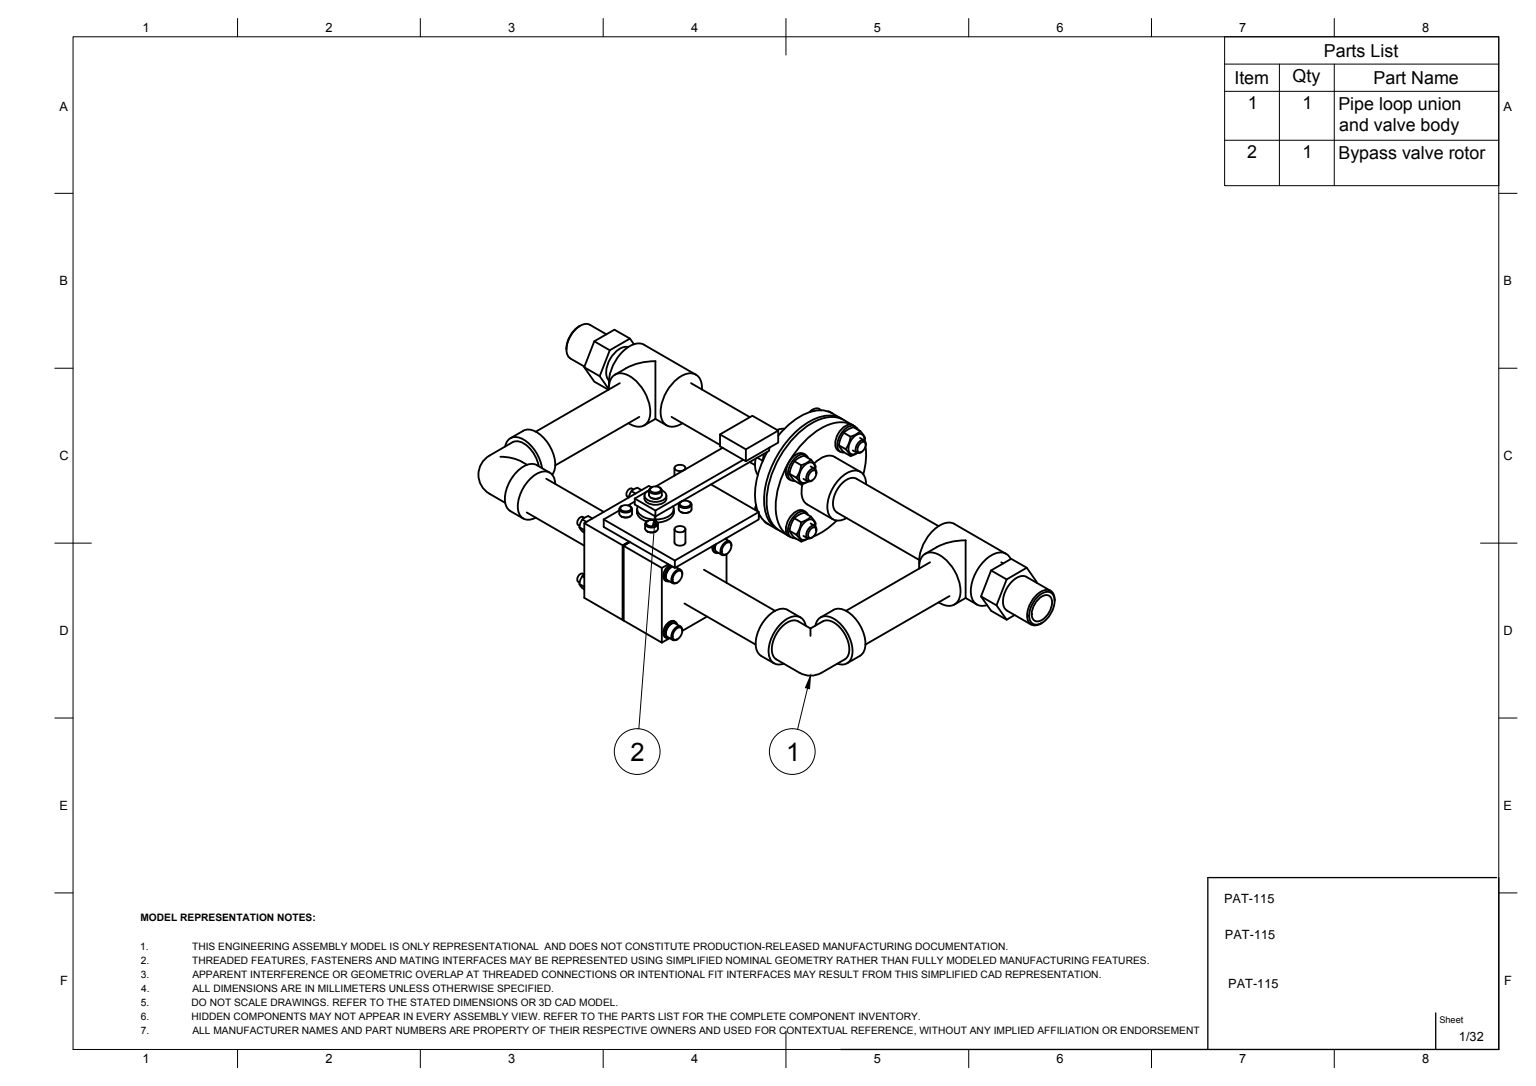
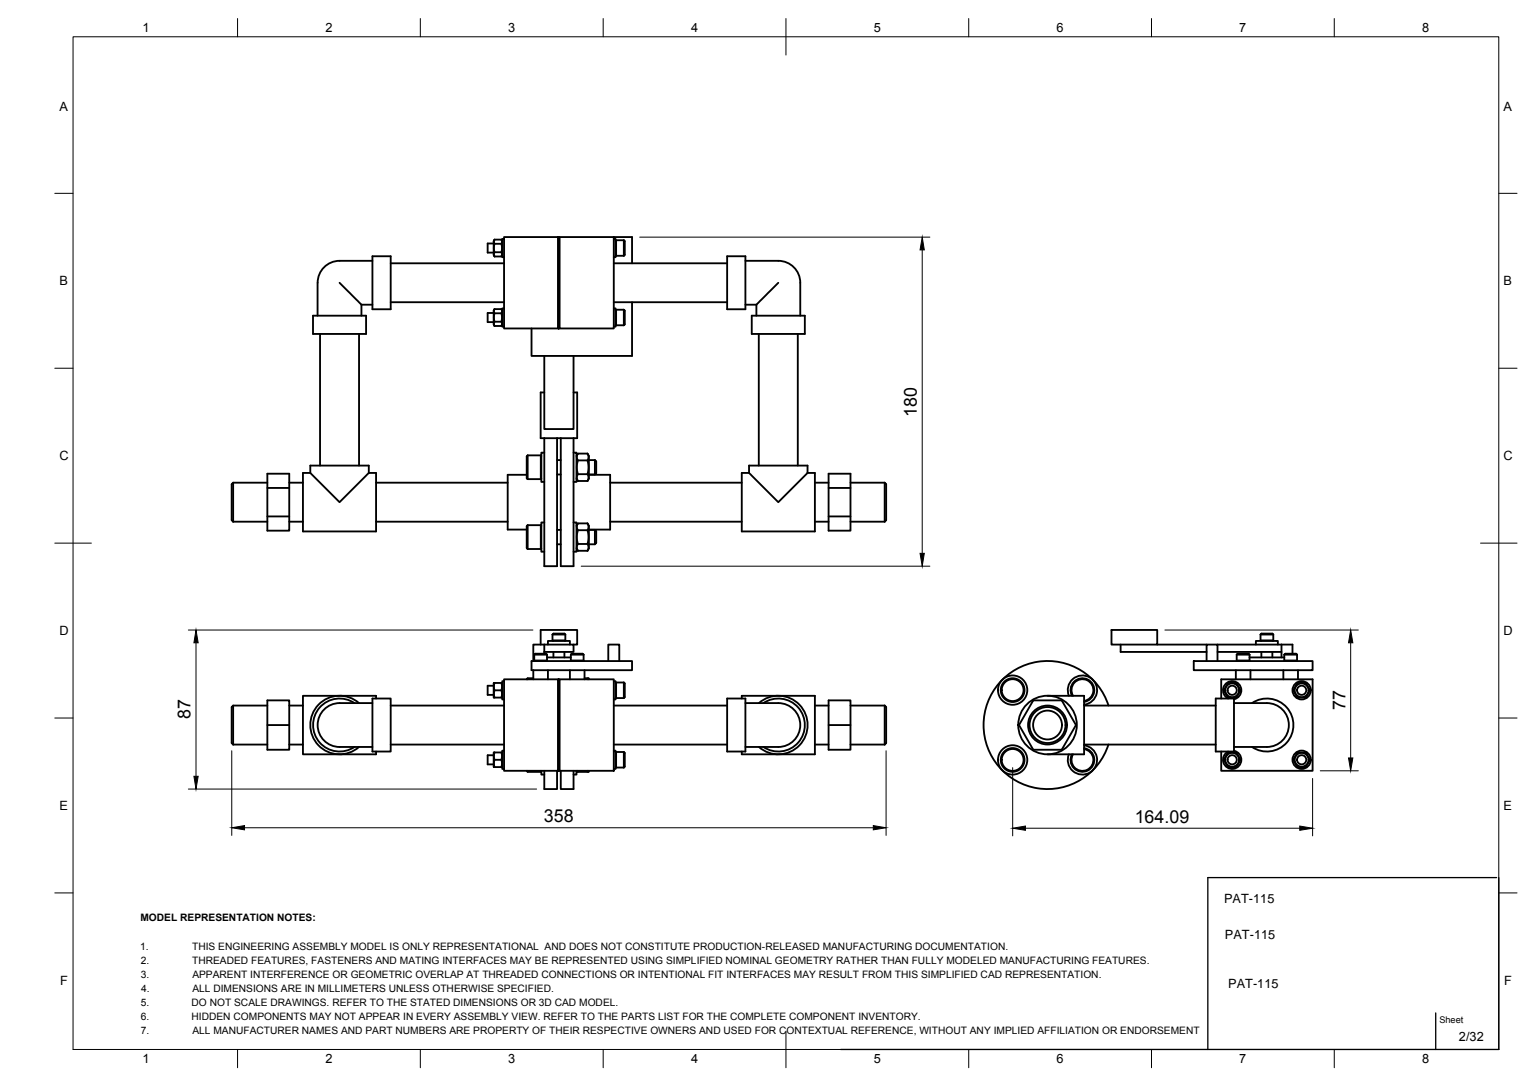
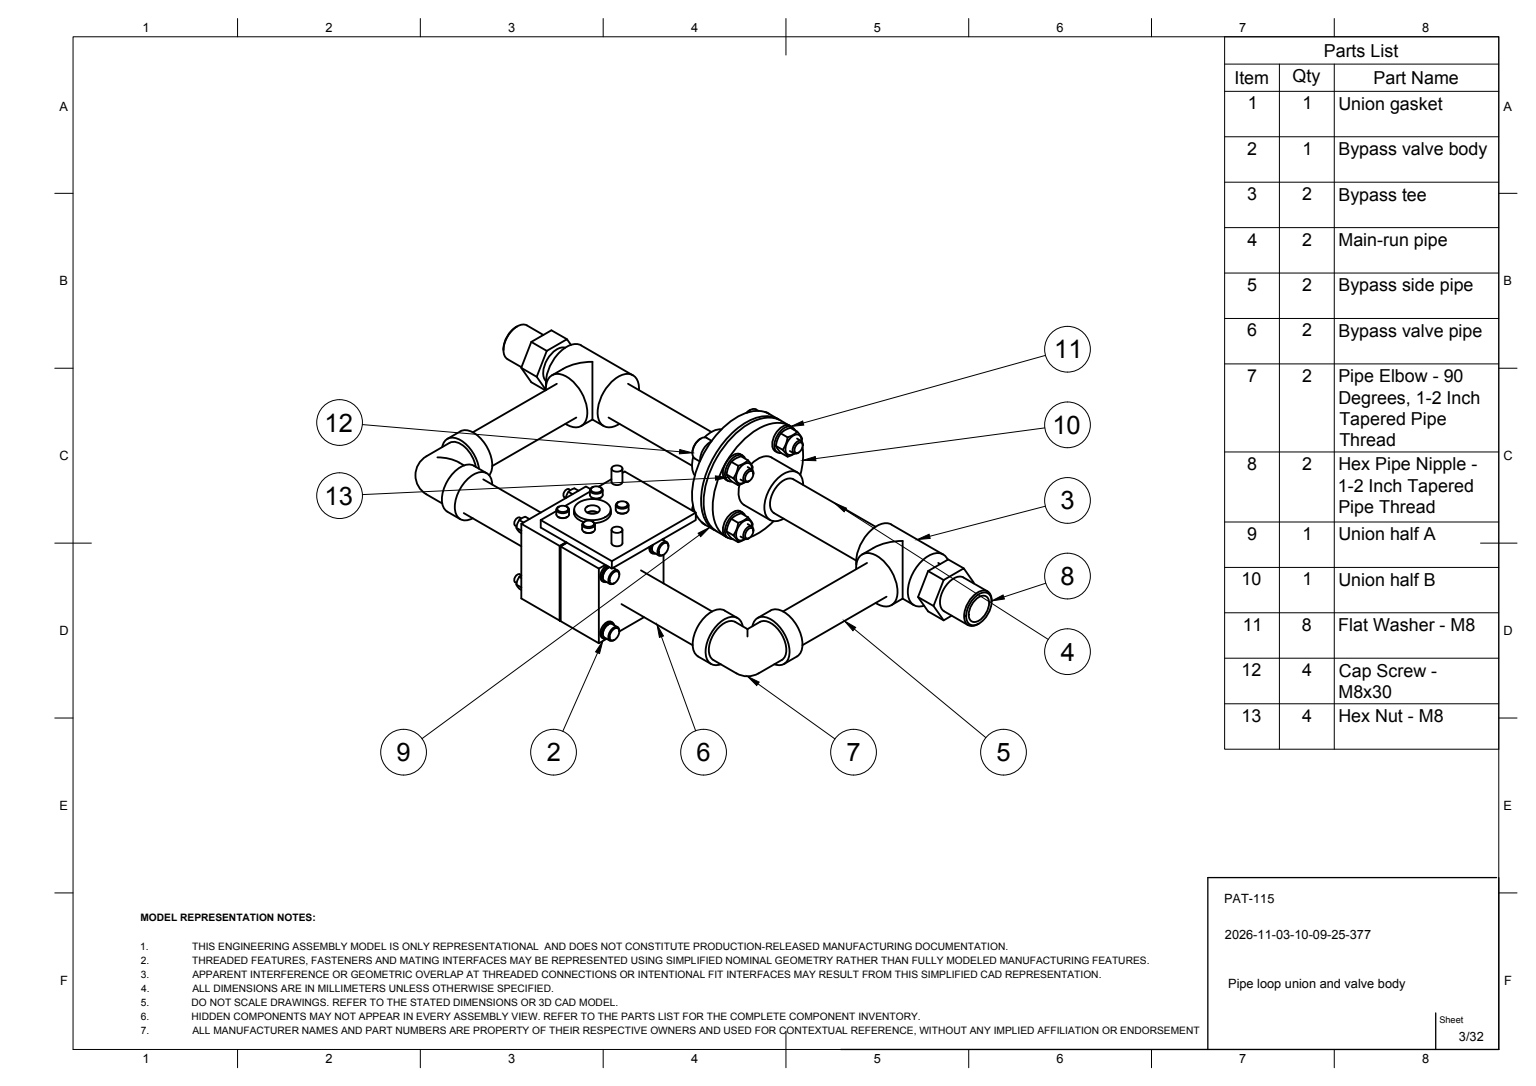
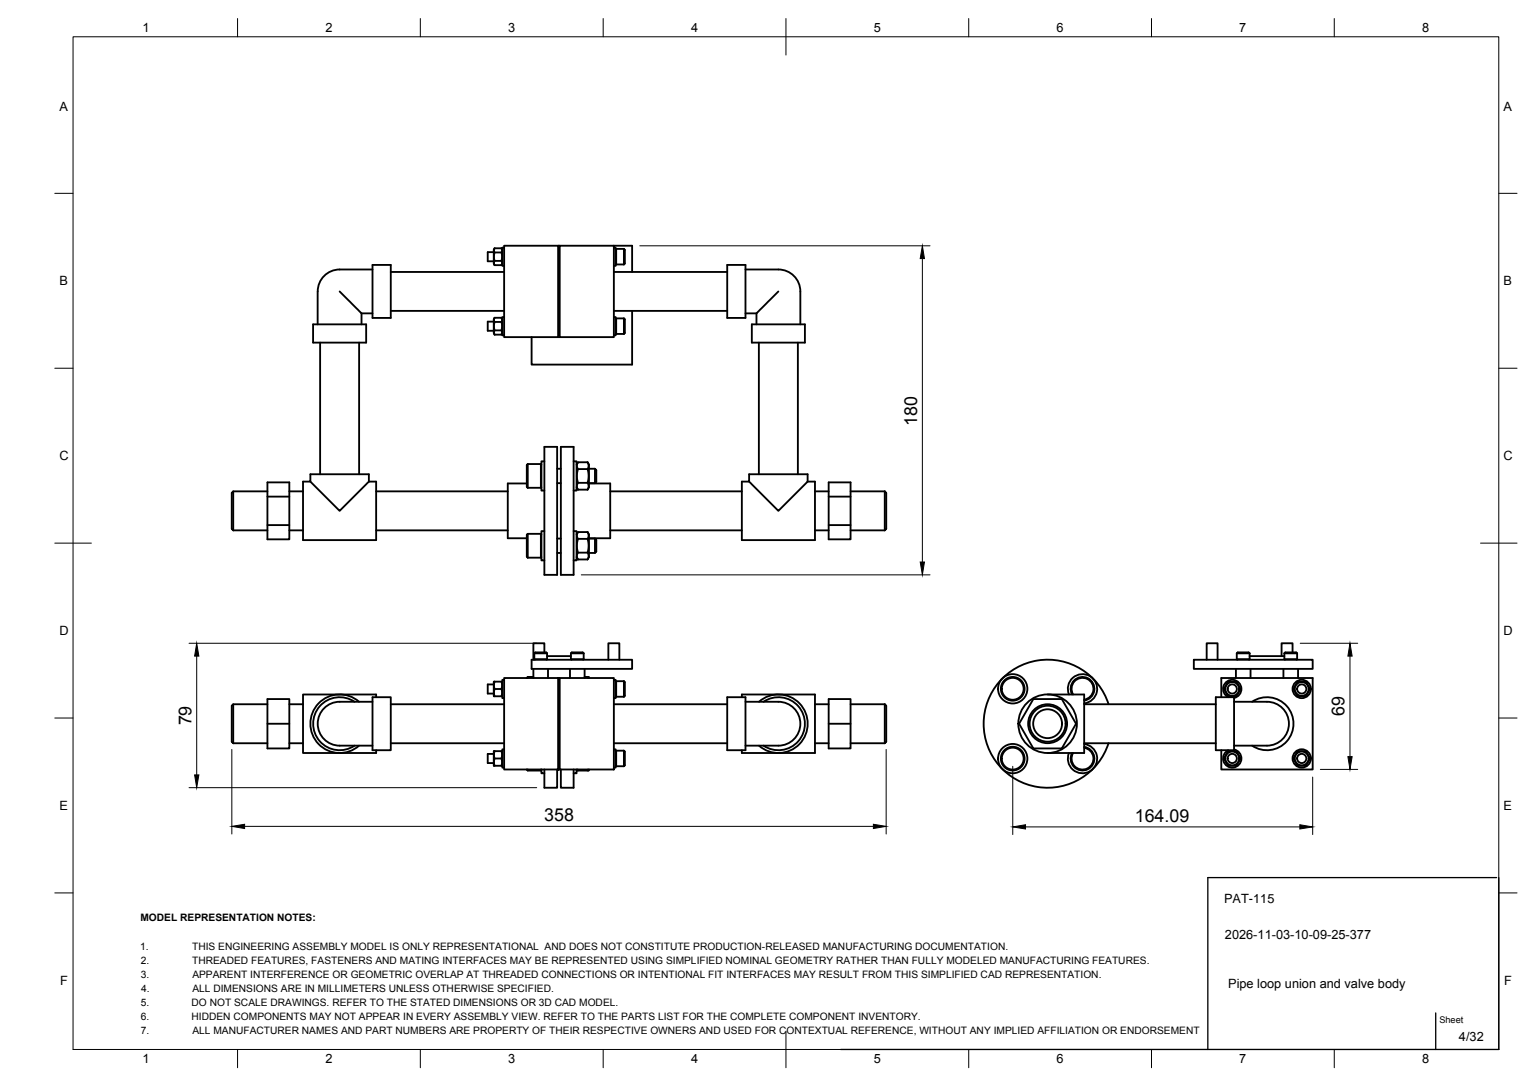
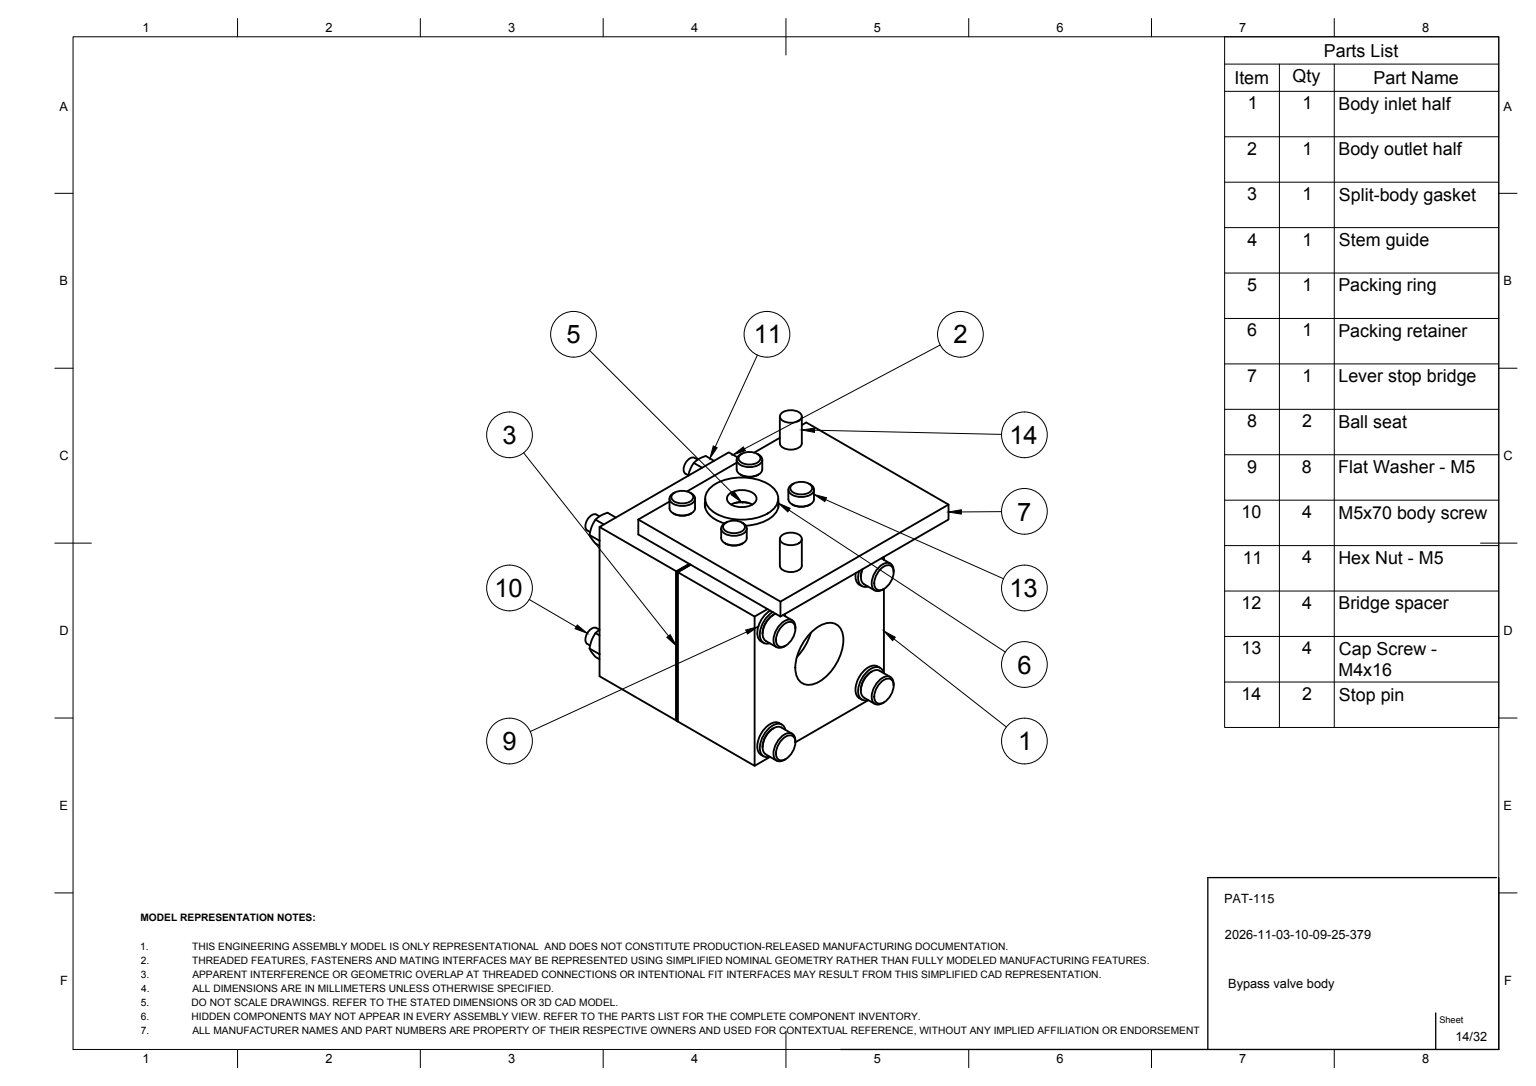
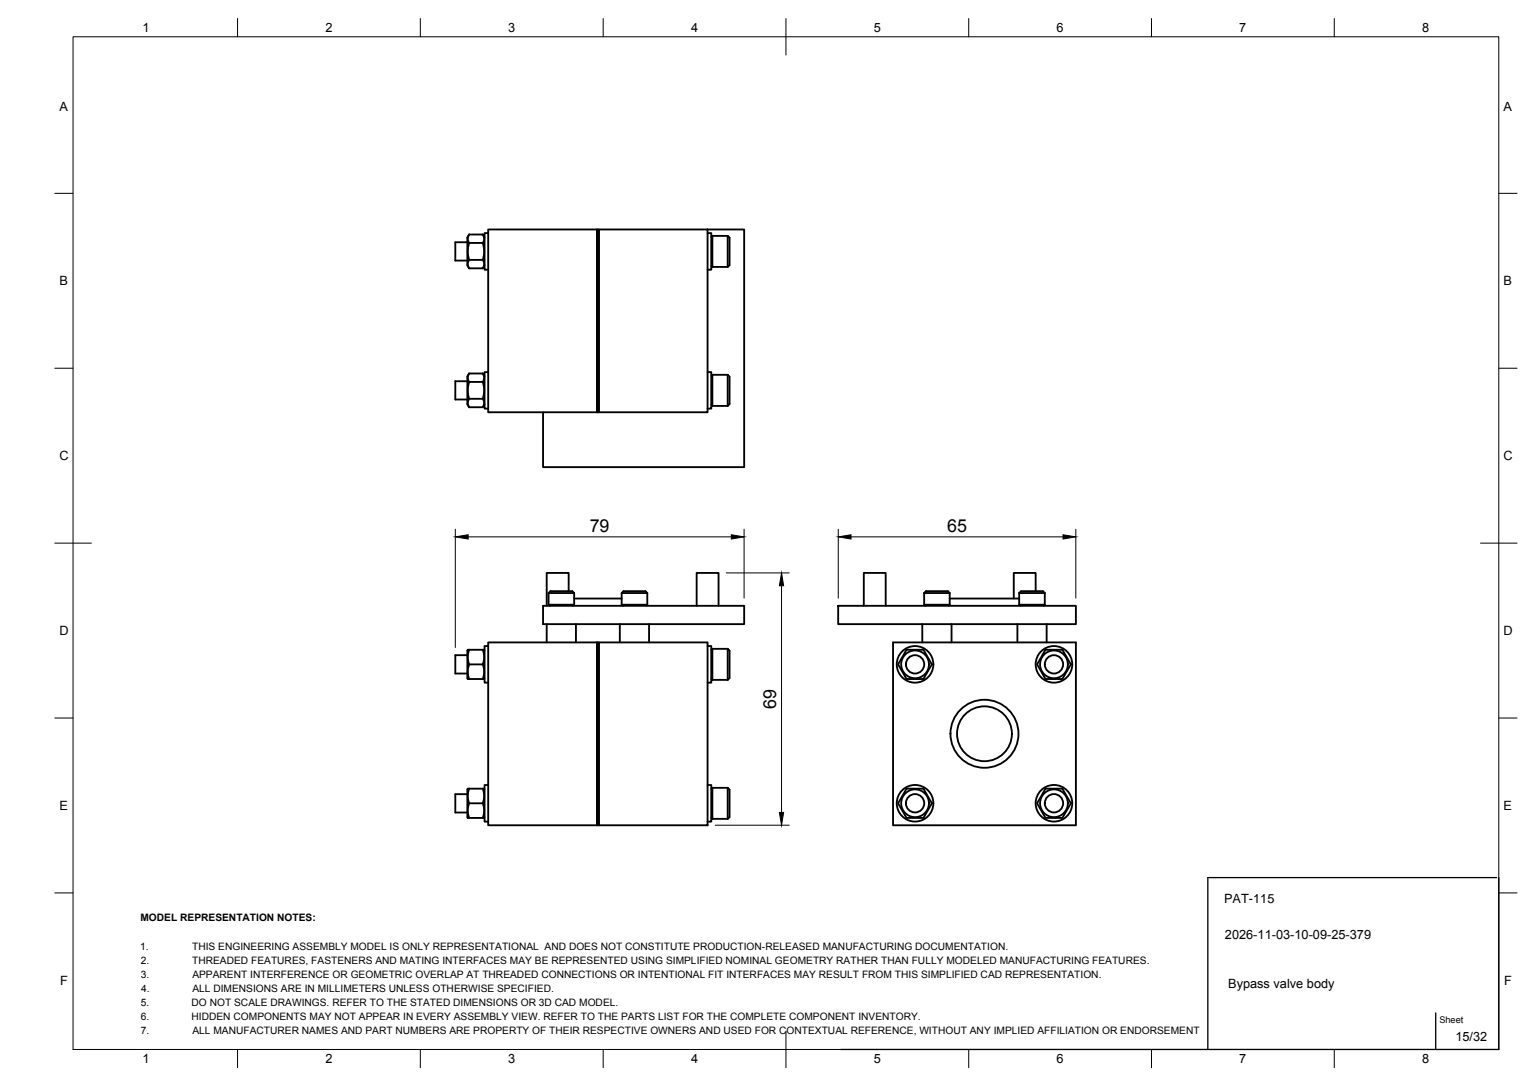
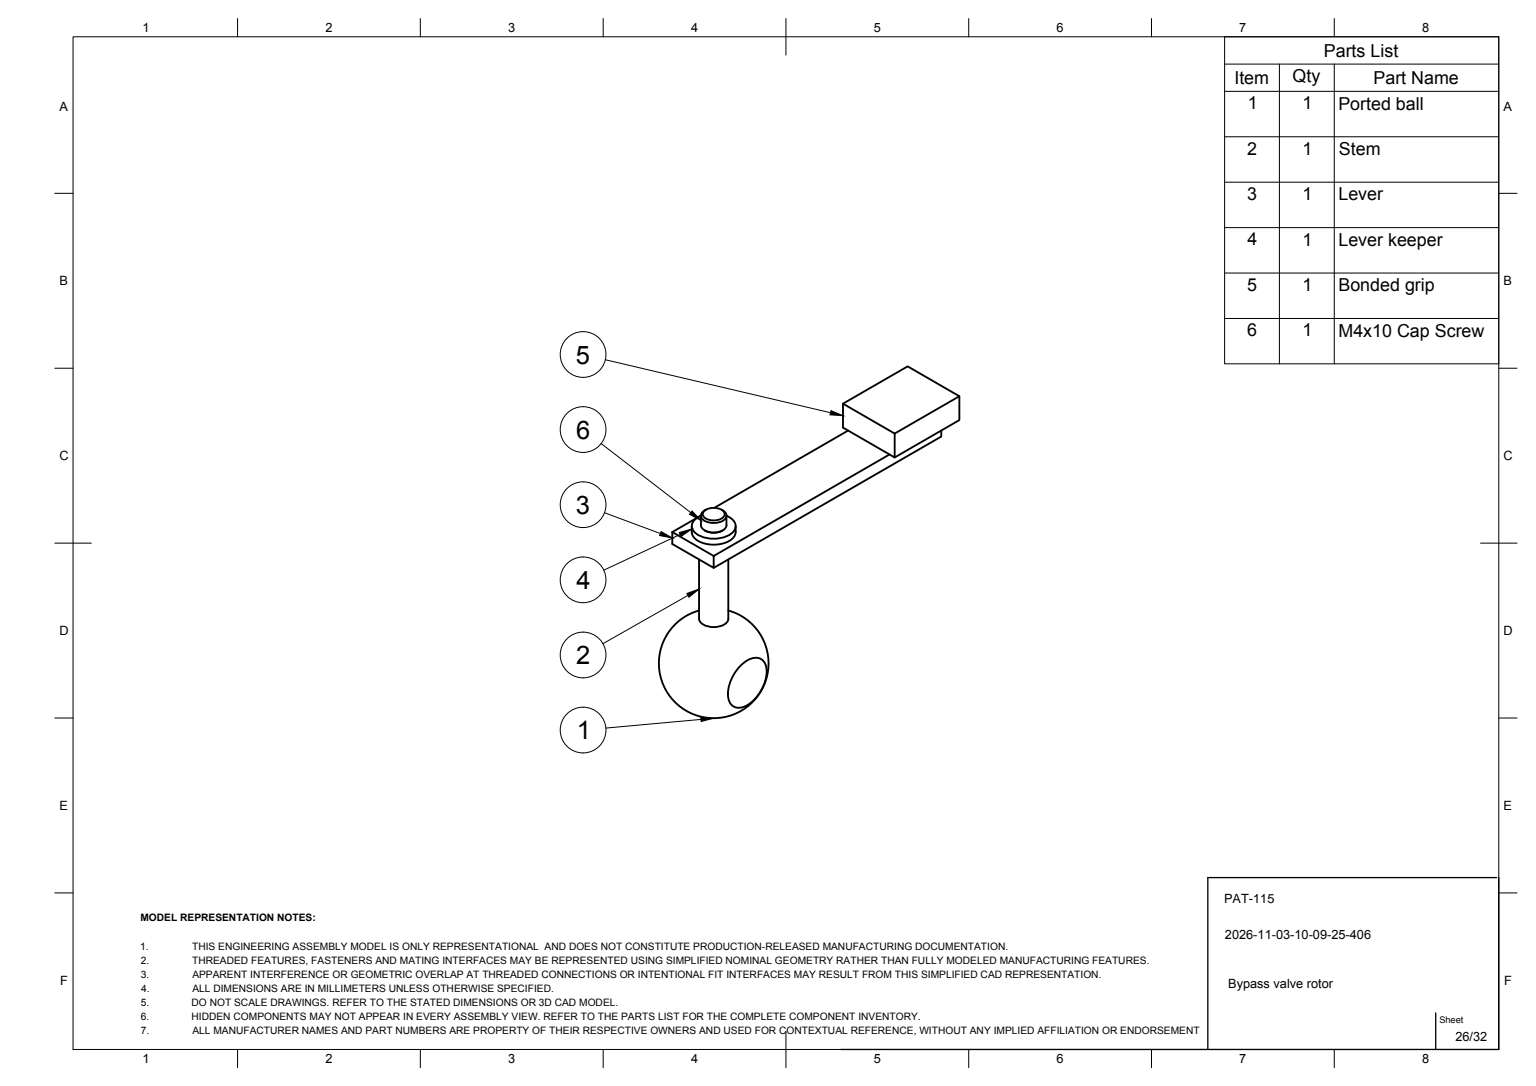
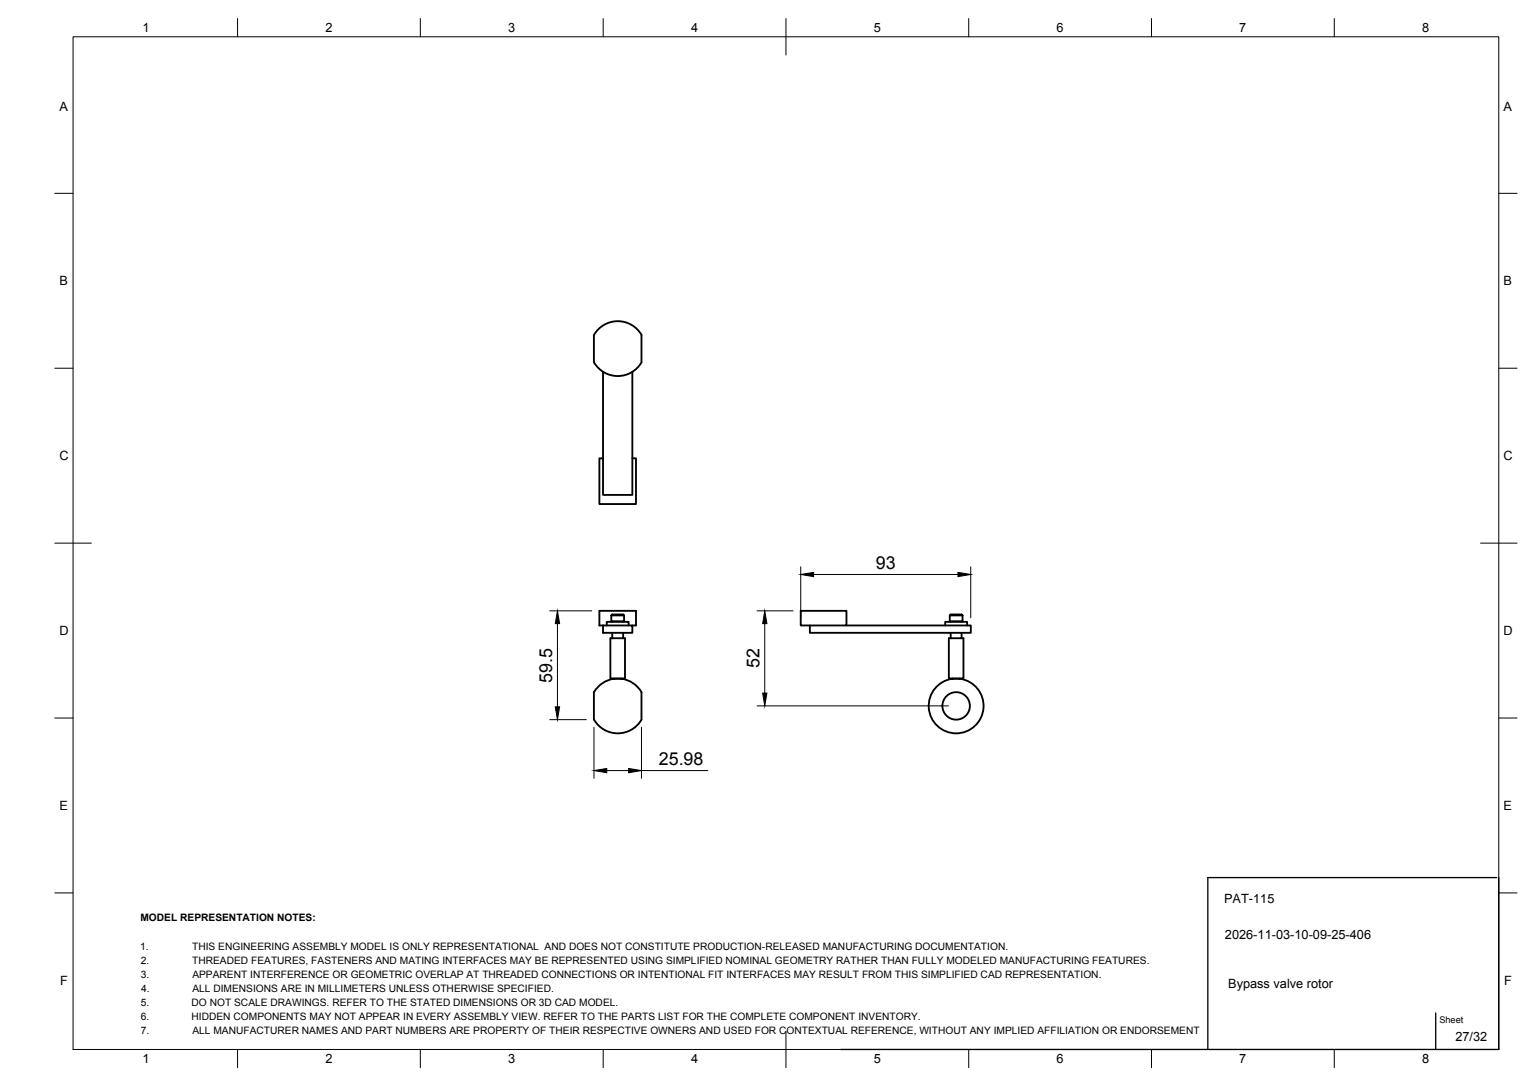
ISO-10303-21;
HEADER;
/* Generated by software containing ST-Developer
 * from STEP Tools, Inc. (www.steptools.com) 
 */

FILE_DESCRIPTION(
/* description */ ('Union bypass pipe loop'),
/* implementation_level */ '2;1');

FILE_NAME(
/* name */ 'PAT-115',
/* time_stamp */ '2026-10-27T21:00:29-07:00',
/* author */ (''),
/* organization */ (''),
/* preprocessor_version */ 'ST-DEVELOPER v20.2',
/* originating_system */ 'Autodesk Translation Framework v15.17.0.0',
/* authorisation */ '');

FILE_SCHEMA (('AUTOMOTIVE_DESIGN { 1 0 10303 214 3 1 1 }'));
ENDSEC;

DATA;
#10=MECHANICAL_DESIGN_GEOMETRIC_PRESENTATION_REPRESENTATION('',(#445,#446,
#447,#448,#449,#450,#451,#452,#453,#454,#455,#456,#457,#458,#459,#460,#461,
#462,#463,#464,#465,#466,#467,#468,#469,#470,#471,#472,#473,#474,#475,#476),
#10095);
#11=ELLIPSE('',#6238,1.31521861300698,0.93);
#12=ELLIPSE('',#6239,1.31521861300698,0.93);
#13=ELLIPSE('',#6241,1.31521861300698,0.93);
#14=ELLIPSE('',#6249,1.11722871427474,0.789999999999999);
#15=ELLIPSE('',#6250,1.11722871427474,0.789999999999999);
#16=ELLIPSE('',#6254,1.11722871427474,0.789999999999999);
#17=ELLIPSE('',#6255,1.11722871427474,0.789999999999999);
#18=ELLIPSE('',#6263,1.11722871427474,0.789999999999999);
#19=ELLIPSE('',#6264,1.11722871427474,0.789999999999999);
#20=ELLIPSE('',#6265,1.11722871427474,0.789999999999999);
#21=ELLIPSE('',#6266,1.11722871427474,0.789999999999999);
#22=ELLIPSE('',#6274,2.26274169979695,1.6);
#23=ELLIPSE('',#6275,2.26274169979695,1.6);
#24=ELLIPSE('',#6277,2.26274169979695,1.6);
#25=ELLIPSE('',#6313,1.11722871427475,0.79);
#26=ELLIPSE('',#6337,1.69705627484771,1.2);
#27=ITEM_DEFINED_TRANSFORMATION($,$,#5908,#6188);
#28=ITEM_DEFINED_TRANSFORMATION($,$,#5951,#6189);
#29=ITEM_DEFINED_TRANSFORMATION($,$,#5994,#6190);
#30=ITEM_DEFINED_TRANSFORMATION($,$,#6021,#6191);
#31=ITEM_DEFINED_TRANSFORMATION($,$,#6034,#6192);
#32=ITEM_DEFINED_TRANSFORMATION($,$,#6038,#6193);
#33=ITEM_DEFINED_TRANSFORMATION($,$,#6051,#6194);
#34=ITEM_DEFINED_TRANSFORMATION($,$,#6081,#6195);
#35=ITEM_DEFINED_TRANSFORMATION($,$,#6081,#6196);
#36=ITEM_DEFINED_TRANSFORMATION($,$,#6120,#6197);
#37=ITEM_DEFINED_TRANSFORMATION($,$,#6092,#6198);
#38=ITEM_DEFINED_TRANSFORMATION($,$,#6120,#6199);
#39=ITEM_DEFINED_TRANSFORMATION($,$,#6131,#6200);
#40=ITEM_DEFINED_TRANSFORMATION($,$,#6120,#6201);
#41=ITEM_DEFINED_TRANSFORMATION($,$,#6092,#6202);
#42=ITEM_DEFINED_TRANSFORMATION($,$,#6120,#6203);
#43=ITEM_DEFINED_TRANSFORMATION($,$,#6131,#6204);
#44=ITEM_DEFINED_TRANSFORMATION($,$,#6120,#6205);
#45=ITEM_DEFINED_TRANSFORMATION($,$,#6092,#6206);
#46=ITEM_DEFINED_TRANSFORMATION($,$,#6120,#6207);
#47=ITEM_DEFINED_TRANSFORMATION($,$,#6131,#6208);
#48=ITEM_DEFINED_TRANSFORMATION($,$,#6120,#6209);
#49=ITEM_DEFINED_TRANSFORMATION($,$,#6092,#6210);
#50=ITEM_DEFINED_TRANSFORMATION($,$,#6120,#6211);
#51=ITEM_DEFINED_TRANSFORMATION($,$,#6131,#6212);
#52=ITEM_DEFINED_TRANSFORMATION($,$,#6147,#6213);
#53=ITEM_DEFINED_TRANSFORMATION($,$,#6156,#6214);
#54=ITEM_DEFINED_TRANSFORMATION($,$,#6147,#6215);
#55=ITEM_DEFINED_TRANSFORMATION($,$,#6156,#6216);
#56=ITEM_DEFINED_TRANSFORMATION($,$,#6147,#6217);
#57=ITEM_DEFINED_TRANSFORMATION($,$,#6156,#6218);
#58=ITEM_DEFINED_TRANSFORMATION($,$,#6147,#6219);
#59=ITEM_DEFINED_TRANSFORMATION($,$,#6156,#6220);
#60=ITEM_DEFINED_TRANSFORMATION($,$,#6182,#6221);
#61=ITEM_DEFINED_TRANSFORMATION($,$,#6182,#6222);
#62=ITEM_DEFINED_TRANSFORMATION($,$,#5907,#6476);
#63=ITEM_DEFINED_TRANSFORMATION($,$,#6223,#6477);
#64=ITEM_DEFINED_TRANSFORMATION($,$,#6232,#6478);
#65=ITEM_DEFINED_TRANSFORMATION($,$,#6284,#6479);
#66=ITEM_DEFINED_TRANSFORMATION($,$,#6293,#6480);
#67=ITEM_DEFINED_TRANSFORMATION($,$,#6302,#6481);
#68=ITEM_DEFINED_TRANSFORMATION($,$,#6232,#6482);
#69=ITEM_DEFINED_TRANSFORMATION($,$,#6284,#6483);
#70=ITEM_DEFINED_TRANSFORMATION($,$,#6293,#6484);
#71=ITEM_DEFINED_TRANSFORMATION($,$,#6302,#6485);
#72=ITEM_DEFINED_TRANSFORMATION($,$,#6311,#6486);
#73=ITEM_DEFINED_TRANSFORMATION($,$,#6311,#6487);
#74=ITEM_DEFINED_TRANSFORMATION($,$,#6351,#6488);
#75=ITEM_DEFINED_TRANSFORMATION($,$,#6351,#6489);
#76=ITEM_DEFINED_TRANSFORMATION($,$,#6375,#6490);
#77=ITEM_DEFINED_TRANSFORMATION($,$,#6400,#6491);
#78=ITEM_DEFINED_TRANSFORMATION($,$,#6451,#6492);
#79=ITEM_DEFINED_TRANSFORMATION($,$,#6425,#6493);
#80=ITEM_DEFINED_TRANSFORMATION($,$,#6451,#6494);
#81=ITEM_DEFINED_TRANSFORMATION($,$,#6460,#6495);
#82=ITEM_DEFINED_TRANSFORMATION($,$,#6451,#6496);
#83=ITEM_DEFINED_TRANSFORMATION($,$,#6425,#6497);
#84=ITEM_DEFINED_TRANSFORMATION($,$,#6451,#6498);
#85=ITEM_DEFINED_TRANSFORMATION($,$,#6460,#6499);
#86=ITEM_DEFINED_TRANSFORMATION($,$,#6451,#6500);
#87=ITEM_DEFINED_TRANSFORMATION($,$,#6425,#6501);
#88=ITEM_DEFINED_TRANSFORMATION($,$,#6451,#6502);
#89=ITEM_DEFINED_TRANSFORMATION($,$,#6460,#6503);
#90=ITEM_DEFINED_TRANSFORMATION($,$,#6451,#6504);
#91=ITEM_DEFINED_TRANSFORMATION($,$,#6425,#6505);
#92=ITEM_DEFINED_TRANSFORMATION($,$,#6451,#6506);
#93=ITEM_DEFINED_TRANSFORMATION($,$,#6460,#6507);
#94=ITEM_DEFINED_TRANSFORMATION($,$,#6509,#6611);
#95=ITEM_DEFINED_TRANSFORMATION($,$,#6525,#6612);
#96=ITEM_DEFINED_TRANSFORMATION($,$,#6560,#6613);
#97=ITEM_DEFINED_TRANSFORMATION($,$,#6571,#6614);
#98=ITEM_DEFINED_TRANSFORMATION($,$,#6580,#6615);
#99=ITEM_DEFINED_TRANSFORMATION($,$,#6587,#6616);
#100=ITEM_DEFINED_TRANSFORMATION($,$,#5906,#6617);
#101=ITEM_DEFINED_TRANSFORMATION($,$,#6508,#6618);
#102=(
REPRESENTATION_RELATIONSHIP($,$,#10250,#10249)
REPRESENTATION_RELATIONSHIP_WITH_TRANSFORMATION(#27)
SHAPE_REPRESENTATION_RELATIONSHIP()
);
#103=(
REPRESENTATION_RELATIONSHIP($,$,#10251,#10249)
REPRESENTATION_RELATIONSHIP_WITH_TRANSFORMATION(#28)
SHAPE_REPRESENTATION_RELATIONSHIP()
);
#104=(
REPRESENTATION_RELATIONSHIP($,$,#10252,#10249)
REPRESENTATION_RELATIONSHIP_WITH_TRANSFORMATION(#29)
SHAPE_REPRESENTATION_RELATIONSHIP()
);
#105=(
REPRESENTATION_RELATIONSHIP($,$,#10253,#10249)
REPRESENTATION_RELATIONSHIP_WITH_TRANSFORMATION(#30)
SHAPE_REPRESENTATION_RELATIONSHIP()
);
#106=(
REPRESENTATION_RELATIONSHIP($,$,#10254,#10249)
REPRESENTATION_RELATIONSHIP_WITH_TRANSFORMATION(#31)
SHAPE_REPRESENTATION_RELATIONSHIP()
);
#107=(
REPRESENTATION_RELATIONSHIP($,$,#10255,#10249)
REPRESENTATION_RELATIONSHIP_WITH_TRANSFORMATION(#32)
SHAPE_REPRESENTATION_RELATIONSHIP()
);
#108=(
REPRESENTATION_RELATIONSHIP($,$,#10256,#10249)
REPRESENTATION_RELATIONSHIP_WITH_TRANSFORMATION(#33)
SHAPE_REPRESENTATION_RELATIONSHIP()
);
#109=(
REPRESENTATION_RELATIONSHIP($,$,#10257,#10249)
REPRESENTATION_RELATIONSHIP_WITH_TRANSFORMATION(#34)
SHAPE_REPRESENTATION_RELATIONSHIP()
);
#110=(
REPRESENTATION_RELATIONSHIP($,$,#10257,#10249)
REPRESENTATION_RELATIONSHIP_WITH_TRANSFORMATION(#35)
SHAPE_REPRESENTATION_RELATIONSHIP()
);
#111=(
REPRESENTATION_RELATIONSHIP($,$,#10259,#10249)
REPRESENTATION_RELATIONSHIP_WITH_TRANSFORMATION(#36)
SHAPE_REPRESENTATION_RELATIONSHIP()
);
#112=(
REPRESENTATION_RELATIONSHIP($,$,#10258,#10249)
REPRESENTATION_RELATIONSHIP_WITH_TRANSFORMATION(#37)
SHAPE_REPRESENTATION_RELATIONSHIP()
);
#113=(
REPRESENTATION_RELATIONSHIP($,$,#10259,#10249)
REPRESENTATION_RELATIONSHIP_WITH_TRANSFORMATION(#38)
SHAPE_REPRESENTATION_RELATIONSHIP()
);
#114=(
REPRESENTATION_RELATIONSHIP($,$,#10260,#10249)
REPRESENTATION_RELATIONSHIP_WITH_TRANSFORMATION(#39)
SHAPE_REPRESENTATION_RELATIONSHIP()
);
#115=(
REPRESENTATION_RELATIONSHIP($,$,#10259,#10249)
REPRESENTATION_RELATIONSHIP_WITH_TRANSFORMATION(#40)
SHAPE_REPRESENTATION_RELATIONSHIP()
);
#116=(
REPRESENTATION_RELATIONSHIP($,$,#10258,#10249)
REPRESENTATION_RELATIONSHIP_WITH_TRANSFORMATION(#41)
SHAPE_REPRESENTATION_RELATIONSHIP()
);
#117=(
REPRESENTATION_RELATIONSHIP($,$,#10259,#10249)
REPRESENTATION_RELATIONSHIP_WITH_TRANSFORMATION(#42)
SHAPE_REPRESENTATION_RELATIONSHIP()
);
#118=(
REPRESENTATION_RELATIONSHIP($,$,#10260,#10249)
REPRESENTATION_RELATIONSHIP_WITH_TRANSFORMATION(#43)
SHAPE_REPRESENTATION_RELATIONSHIP()
);
#119=(
REPRESENTATION_RELATIONSHIP($,$,#10259,#10249)
REPRESENTATION_RELATIONSHIP_WITH_TRANSFORMATION(#44)
SHAPE_REPRESENTATION_RELATIONSHIP()
);
#120=(
REPRESENTATION_RELATIONSHIP($,$,#10258,#10249)
REPRESENTATION_RELATIONSHIP_WITH_TRANSFORMATION(#45)
SHAPE_REPRESENTATION_RELATIONSHIP()
);
#121=(
REPRESENTATION_RELATIONSHIP($,$,#10259,#10249)
REPRESENTATION_RELATIONSHIP_WITH_TRANSFORMATION(#46)
SHAPE_REPRESENTATION_RELATIONSHIP()
);
#122=(
REPRESENTATION_RELATIONSHIP($,$,#10260,#10249)
REPRESENTATION_RELATIONSHIP_WITH_TRANSFORMATION(#47)
SHAPE_REPRESENTATION_RELATIONSHIP()
);
#123=(
REPRESENTATION_RELATIONSHIP($,$,#10259,#10249)
REPRESENTATION_RELATIONSHIP_WITH_TRANSFORMATION(#48)
SHAPE_REPRESENTATION_RELATIONSHIP()
);
#124=(
REPRESENTATION_RELATIONSHIP($,$,#10258,#10249)
REPRESENTATION_RELATIONSHIP_WITH_TRANSFORMATION(#49)
SHAPE_REPRESENTATION_RELATIONSHIP()
);
#125=(
REPRESENTATION_RELATIONSHIP($,$,#10259,#10249)
REPRESENTATION_RELATIONSHIP_WITH_TRANSFORMATION(#50)
SHAPE_REPRESENTATION_RELATIONSHIP()
);
#126=(
REPRESENTATION_RELATIONSHIP($,$,#10260,#10249)
REPRESENTATION_RELATIONSHIP_WITH_TRANSFORMATION(#51)
SHAPE_REPRESENTATION_RELATIONSHIP()
);
#127=(
REPRESENTATION_RELATIONSHIP($,$,#10261,#10249)
REPRESENTATION_RELATIONSHIP_WITH_TRANSFORMATION(#52)
SHAPE_REPRESENTATION_RELATIONSHIP()
);
#128=(
REPRESENTATION_RELATIONSHIP($,$,#10262,#10249)
REPRESENTATION_RELATIONSHIP_WITH_TRANSFORMATION(#53)
SHAPE_REPRESENTATION_RELATIONSHIP()
);
#129=(
REPRESENTATION_RELATIONSHIP($,$,#10261,#10249)
REPRESENTATION_RELATIONSHIP_WITH_TRANSFORMATION(#54)
SHAPE_REPRESENTATION_RELATIONSHIP()
);
#130=(
REPRESENTATION_RELATIONSHIP($,$,#10262,#10249)
REPRESENTATION_RELATIONSHIP_WITH_TRANSFORMATION(#55)
SHAPE_REPRESENTATION_RELATIONSHIP()
);
#131=(
REPRESENTATION_RELATIONSHIP($,$,#10261,#10249)
REPRESENTATION_RELATIONSHIP_WITH_TRANSFORMATION(#56)
SHAPE_REPRESENTATION_RELATIONSHIP()
);
#132=(
REPRESENTATION_RELATIONSHIP($,$,#10262,#10249)
REPRESENTATION_RELATIONSHIP_WITH_TRANSFORMATION(#57)
SHAPE_REPRESENTATION_RELATIONSHIP()
);
#133=(
REPRESENTATION_RELATIONSHIP($,$,#10261,#10249)
REPRESENTATION_RELATIONSHIP_WITH_TRANSFORMATION(#58)
SHAPE_REPRESENTATION_RELATIONSHIP()
);
#134=(
REPRESENTATION_RELATIONSHIP($,$,#10262,#10249)
REPRESENTATION_RELATIONSHIP_WITH_TRANSFORMATION(#59)
SHAPE_REPRESENTATION_RELATIONSHIP()
);
#135=(
REPRESENTATION_RELATIONSHIP($,$,#10263,#10249)
REPRESENTATION_RELATIONSHIP_WITH_TRANSFORMATION(#60)
SHAPE_REPRESENTATION_RELATIONSHIP()
);
#136=(
REPRESENTATION_RELATIONSHIP($,$,#10263,#10249)
REPRESENTATION_RELATIONSHIP_WITH_TRANSFORMATION(#61)
SHAPE_REPRESENTATION_RELATIONSHIP()
);
#137=(
REPRESENTATION_RELATIONSHIP($,$,#10249,#10248)
REPRESENTATION_RELATIONSHIP_WITH_TRANSFORMATION(#62)
SHAPE_REPRESENTATION_RELATIONSHIP()
);
#138=(
REPRESENTATION_RELATIONSHIP($,$,#10264,#10248)
REPRESENTATION_RELATIONSHIP_WITH_TRANSFORMATION(#63)
SHAPE_REPRESENTATION_RELATIONSHIP()
);
#139=(
REPRESENTATION_RELATIONSHIP($,$,#10265,#10248)
REPRESENTATION_RELATIONSHIP_WITH_TRANSFORMATION(#64)
SHAPE_REPRESENTATION_RELATIONSHIP()
);
#140=(
REPRESENTATION_RELATIONSHIP($,$,#10266,#10248)
REPRESENTATION_RELATIONSHIP_WITH_TRANSFORMATION(#65)
SHAPE_REPRESENTATION_RELATIONSHIP()
);
#141=(
REPRESENTATION_RELATIONSHIP($,$,#10267,#10248)
REPRESENTATION_RELATIONSHIP_WITH_TRANSFORMATION(#66)
SHAPE_REPRESENTATION_RELATIONSHIP()
);
#142=(
REPRESENTATION_RELATIONSHIP($,$,#10268,#10248)
REPRESENTATION_RELATIONSHIP_WITH_TRANSFORMATION(#67)
SHAPE_REPRESENTATION_RELATIONSHIP()
);
#143=(
REPRESENTATION_RELATIONSHIP($,$,#10265,#10248)
REPRESENTATION_RELATIONSHIP_WITH_TRANSFORMATION(#68)
SHAPE_REPRESENTATION_RELATIONSHIP()
);
#144=(
REPRESENTATION_RELATIONSHIP($,$,#10266,#10248)
REPRESENTATION_RELATIONSHIP_WITH_TRANSFORMATION(#69)
SHAPE_REPRESENTATION_RELATIONSHIP()
);
#145=(
REPRESENTATION_RELATIONSHIP($,$,#10267,#10248)
REPRESENTATION_RELATIONSHIP_WITH_TRANSFORMATION(#70)
SHAPE_REPRESENTATION_RELATIONSHIP()
);
#146=(
REPRESENTATION_RELATIONSHIP($,$,#10268,#10248)
REPRESENTATION_RELATIONSHIP_WITH_TRANSFORMATION(#71)
SHAPE_REPRESENTATION_RELATIONSHIP()
);
#147=(
REPRESENTATION_RELATIONSHIP($,$,#10269,#10248)
REPRESENTATION_RELATIONSHIP_WITH_TRANSFORMATION(#72)
SHAPE_REPRESENTATION_RELATIONSHIP()
);
#148=(
REPRESENTATION_RELATIONSHIP($,$,#10269,#10248)
REPRESENTATION_RELATIONSHIP_WITH_TRANSFORMATION(#73)
SHAPE_REPRESENTATION_RELATIONSHIP()
);
#149=(
REPRESENTATION_RELATIONSHIP($,$,#10270,#10248)
REPRESENTATION_RELATIONSHIP_WITH_TRANSFORMATION(#74)
SHAPE_REPRESENTATION_RELATIONSHIP()
);
#150=(
REPRESENTATION_RELATIONSHIP($,$,#10270,#10248)
REPRESENTATION_RELATIONSHIP_WITH_TRANSFORMATION(#75)
SHAPE_REPRESENTATION_RELATIONSHIP()
);
#151=(
REPRESENTATION_RELATIONSHIP($,$,#10271,#10248)
REPRESENTATION_RELATIONSHIP_WITH_TRANSFORMATION(#76)
SHAPE_REPRESENTATION_RELATIONSHIP()
);
#152=(
REPRESENTATION_RELATIONSHIP($,$,#10272,#10248)
REPRESENTATION_RELATIONSHIP_WITH_TRANSFORMATION(#77)
SHAPE_REPRESENTATION_RELATIONSHIP()
);
#153=(
REPRESENTATION_RELATIONSHIP($,$,#10274,#10248)
REPRESENTATION_RELATIONSHIP_WITH_TRANSFORMATION(#78)
SHAPE_REPRESENTATION_RELATIONSHIP()
);
#154=(
REPRESENTATION_RELATIONSHIP($,$,#10273,#10248)
REPRESENTATION_RELATIONSHIP_WITH_TRANSFORMATION(#79)
SHAPE_REPRESENTATION_RELATIONSHIP()
);
#155=(
REPRESENTATION_RELATIONSHIP($,$,#10274,#10248)
REPRESENTATION_RELATIONSHIP_WITH_TRANSFORMATION(#80)
SHAPE_REPRESENTATION_RELATIONSHIP()
);
#156=(
REPRESENTATION_RELATIONSHIP($,$,#10275,#10248)
REPRESENTATION_RELATIONSHIP_WITH_TRANSFORMATION(#81)
SHAPE_REPRESENTATION_RELATIONSHIP()
);
#157=(
REPRESENTATION_RELATIONSHIP($,$,#10274,#10248)
REPRESENTATION_RELATIONSHIP_WITH_TRANSFORMATION(#82)
SHAPE_REPRESENTATION_RELATIONSHIP()
);
#158=(
REPRESENTATION_RELATIONSHIP($,$,#10273,#10248)
REPRESENTATION_RELATIONSHIP_WITH_TRANSFORMATION(#83)
SHAPE_REPRESENTATION_RELATIONSHIP()
);
#159=(
REPRESENTATION_RELATIONSHIP($,$,#10274,#10248)
REPRESENTATION_RELATIONSHIP_WITH_TRANSFORMATION(#84)
SHAPE_REPRESENTATION_RELATIONSHIP()
);
#160=(
REPRESENTATION_RELATIONSHIP($,$,#10275,#10248)
REPRESENTATION_RELATIONSHIP_WITH_TRANSFORMATION(#85)
SHAPE_REPRESENTATION_RELATIONSHIP()
);
#161=(
REPRESENTATION_RELATIONSHIP($,$,#10274,#10248)
REPRESENTATION_RELATIONSHIP_WITH_TRANSFORMATION(#86)
SHAPE_REPRESENTATION_RELATIONSHIP()
);
#162=(
REPRESENTATION_RELATIONSHIP($,$,#10273,#10248)
REPRESENTATION_RELATIONSHIP_WITH_TRANSFORMATION(#87)
SHAPE_REPRESENTATION_RELATIONSHIP()
);
#163=(
REPRESENTATION_RELATIONSHIP($,$,#10274,#10248)
REPRESENTATION_RELATIONSHIP_WITH_TRANSFORMATION(#88)
SHAPE_REPRESENTATION_RELATIONSHIP()
);
#164=(
REPRESENTATION_RELATIONSHIP($,$,#10275,#10248)
REPRESENTATION_RELATIONSHIP_WITH_TRANSFORMATION(#89)
SHAPE_REPRESENTATION_RELATIONSHIP()
);
#165=(
REPRESENTATION_RELATIONSHIP($,$,#10274,#10248)
REPRESENTATION_RELATIONSHIP_WITH_TRANSFORMATION(#90)
SHAPE_REPRESENTATION_RELATIONSHIP()
);
#166=(
REPRESENTATION_RELATIONSHIP($,$,#10273,#10248)
REPRESENTATION_RELATIONSHIP_WITH_TRANSFORMATION(#91)
SHAPE_REPRESENTATION_RELATIONSHIP()
);
#167=(
REPRESENTATION_RELATIONSHIP($,$,#10274,#10248)
REPRESENTATION_RELATIONSHIP_WITH_TRANSFORMATION(#92)
SHAPE_REPRESENTATION_RELATIONSHIP()
);
#168=(
REPRESENTATION_RELATIONSHIP($,$,#10275,#10248)
REPRESENTATION_RELATIONSHIP_WITH_TRANSFORMATION(#93)
SHAPE_REPRESENTATION_RELATIONSHIP()
);
#169=(
REPRESENTATION_RELATIONSHIP($,$,#10277,#10276)
REPRESENTATION_RELATIONSHIP_WITH_TRANSFORMATION(#94)
SHAPE_REPRESENTATION_RELATIONSHIP()
);
#170=(
REPRESENTATION_RELATIONSHIP($,$,#10278,#10276)
REPRESENTATION_RELATIONSHIP_WITH_TRANSFORMATION(#95)
SHAPE_REPRESENTATION_RELATIONSHIP()
);
#171=(
REPRESENTATION_RELATIONSHIP($,$,#10279,#10276)
REPRESENTATION_RELATIONSHIP_WITH_TRANSFORMATION(#96)
SHAPE_REPRESENTATION_RELATIONSHIP()
);
#172=(
REPRESENTATION_RELATIONSHIP($,$,#10280,#10276)
REPRESENTATION_RELATIONSHIP_WITH_TRANSFORMATION(#97)
SHAPE_REPRESENTATION_RELATIONSHIP()
);
#173=(
REPRESENTATION_RELATIONSHIP($,$,#10281,#10276)
REPRESENTATION_RELATIONSHIP_WITH_TRANSFORMATION(#98)
SHAPE_REPRESENTATION_RELATIONSHIP()
);
#174=(
REPRESENTATION_RELATIONSHIP($,$,#10282,#10276)
REPRESENTATION_RELATIONSHIP_WITH_TRANSFORMATION(#99)
SHAPE_REPRESENTATION_RELATIONSHIP()
);
#175=(
REPRESENTATION_RELATIONSHIP($,$,#10248,#10247)
REPRESENTATION_RELATIONSHIP_WITH_TRANSFORMATION(#100)
SHAPE_REPRESENTATION_RELATIONSHIP()
);
#176=(
REPRESENTATION_RELATIONSHIP($,$,#10276,#10247)
REPRESENTATION_RELATIONSHIP_WITH_TRANSFORMATION(#101)
SHAPE_REPRESENTATION_RELATIONSHIP()
);
#177=CONTEXT_DEPENDENT_SHAPE_REPRESENTATION(#102,#10153);
#178=CONTEXT_DEPENDENT_SHAPE_REPRESENTATION(#103,#10154);
#179=CONTEXT_DEPENDENT_SHAPE_REPRESENTATION(#104,#10155);
#180=CONTEXT_DEPENDENT_SHAPE_REPRESENTATION(#105,#10156);
#181=CONTEXT_DEPENDENT_SHAPE_REPRESENTATION(#106,#10157);
#182=CONTEXT_DEPENDENT_SHAPE_REPRESENTATION(#107,#10158);
#183=CONTEXT_DEPENDENT_SHAPE_REPRESENTATION(#108,#10159);
#184=CONTEXT_DEPENDENT_SHAPE_REPRESENTATION(#109,#10160);
#185=CONTEXT_DEPENDENT_SHAPE_REPRESENTATION(#110,#10161);
#186=CONTEXT_DEPENDENT_SHAPE_REPRESENTATION(#111,#10162);
#187=CONTEXT_DEPENDENT_SHAPE_REPRESENTATION(#112,#10163);
#188=CONTEXT_DEPENDENT_SHAPE_REPRESENTATION(#113,#10164);
#189=CONTEXT_DEPENDENT_SHAPE_REPRESENTATION(#114,#10165);
#190=CONTEXT_DEPENDENT_SHAPE_REPRESENTATION(#115,#10166);
#191=CONTEXT_DEPENDENT_SHAPE_REPRESENTATION(#116,#10167);
#192=CONTEXT_DEPENDENT_SHAPE_REPRESENTATION(#117,#10168);
#193=CONTEXT_DEPENDENT_SHAPE_REPRESENTATION(#118,#10169);
#194=CONTEXT_DEPENDENT_SHAPE_REPRESENTATION(#119,#10170);
#195=CONTEXT_DEPENDENT_SHAPE_REPRESENTATION(#120,#10171);
#196=CONTEXT_DEPENDENT_SHAPE_REPRESENTATION(#121,#10172);
#197=CONTEXT_DEPENDENT_SHAPE_REPRESENTATION(#122,#10173);
#198=CONTEXT_DEPENDENT_SHAPE_REPRESENTATION(#123,#10174);
#199=CONTEXT_DEPENDENT_SHAPE_REPRESENTATION(#124,#10175);
#200=CONTEXT_DEPENDENT_SHAPE_REPRESENTATION(#125,#10176);
#201=CONTEXT_DEPENDENT_SHAPE_REPRESENTATION(#126,#10177);
#202=CONTEXT_DEPENDENT_SHAPE_REPRESENTATION(#127,#10178);
#203=CONTEXT_DEPENDENT_SHAPE_REPRESENTATION(#128,#10179);
#204=CONTEXT_DEPENDENT_SHAPE_REPRESENTATION(#129,#10180);
#205=CONTEXT_DEPENDENT_SHAPE_REPRESENTATION(#130,#10181);
#206=CONTEXT_DEPENDENT_SHAPE_REPRESENTATION(#131,#10182);
#207=CONTEXT_DEPENDENT_SHAPE_REPRESENTATION(#132,#10183);
#208=CONTEXT_DEPENDENT_SHAPE_REPRESENTATION(#133,#10184);
#209=CONTEXT_DEPENDENT_SHAPE_REPRESENTATION(#134,#10185);
#210=CONTEXT_DEPENDENT_SHAPE_REPRESENTATION(#135,#10186);
#211=CONTEXT_DEPENDENT_SHAPE_REPRESENTATION(#136,#10187);
#212=CONTEXT_DEPENDENT_SHAPE_REPRESENTATION(#137,#10200);
#213=CONTEXT_DEPENDENT_SHAPE_REPRESENTATION(#138,#10201);
#214=CONTEXT_DEPENDENT_SHAPE_REPRESENTATION(#139,#10202);
#215=CONTEXT_DEPENDENT_SHAPE_REPRESENTATION(#140,#10203);
#216=CONTEXT_DEPENDENT_SHAPE_REPRESENTATION(#141,#10204);
#217=CONTEXT_DEPENDENT_SHAPE_REPRESENTATION(#142,#10205);
#218=CONTEXT_DEPENDENT_SHAPE_REPRESENTATION(#143,#10206);
#219=CONTEXT_DEPENDENT_SHAPE_REPRESENTATION(#144,#10207);
#220=CONTEXT_DEPENDENT_SHAPE_REPRESENTATION(#145,#10208);
#221=CONTEXT_DEPENDENT_SHAPE_REPRESENTATION(#146,#10209);
#222=CONTEXT_DEPENDENT_SHAPE_REPRESENTATION(#147,#10210);
#223=CONTEXT_DEPENDENT_SHAPE_REPRESENTATION(#148,#10211);
#224=CONTEXT_DEPENDENT_SHAPE_REPRESENTATION(#149,#10212);
#225=CONTEXT_DEPENDENT_SHAPE_REPRESENTATION(#150,#10213);
#226=CONTEXT_DEPENDENT_SHAPE_REPRESENTATION(#151,#10214);
#227=CONTEXT_DEPENDENT_SHAPE_REPRESENTATION(#152,#10215);
#228=CONTEXT_DEPENDENT_SHAPE_REPRESENTATION(#153,#10216);
#229=CONTEXT_DEPENDENT_SHAPE_REPRESENTATION(#154,#10217);
#230=CONTEXT_DEPENDENT_SHAPE_REPRESENTATION(#155,#10218);
#231=CONTEXT_DEPENDENT_SHAPE_REPRESENTATION(#156,#10219);
#232=CONTEXT_DEPENDENT_SHAPE_REPRESENTATION(#157,#10220);
#233=CONTEXT_DEPENDENT_SHAPE_REPRESENTATION(#158,#10221);
#234=CONTEXT_DEPENDENT_SHAPE_REPRESENTATION(#159,#10222);
#235=CONTEXT_DEPENDENT_SHAPE_REPRESENTATION(#160,#10223);
#236=CONTEXT_DEPENDENT_SHAPE_REPRESENTATION(#161,#10224);
#237=CONTEXT_DEPENDENT_SHAPE_REPRESENTATION(#162,#10225);
#238=CONTEXT_DEPENDENT_SHAPE_REPRESENTATION(#163,#10226);
#239=CONTEXT_DEPENDENT_SHAPE_REPRESENTATION(#164,#10227);
#240=CONTEXT_DEPENDENT_SHAPE_REPRESENTATION(#165,#10228);
#241=CONTEXT_DEPENDENT_SHAPE_REPRESENTATION(#166,#10229);
#242=CONTEXT_DEPENDENT_SHAPE_REPRESENTATION(#167,#10230);
#243=CONTEXT_DEPENDENT_SHAPE_REPRESENTATION(#168,#10231);
#244=CONTEXT_DEPENDENT_SHAPE_REPRESENTATION(#169,#10239);
#245=CONTEXT_DEPENDENT_SHAPE_REPRESENTATION(#170,#10240);
#246=CONTEXT_DEPENDENT_SHAPE_REPRESENTATION(#171,#10241);
#247=CONTEXT_DEPENDENT_SHAPE_REPRESENTATION(#172,#10242);
#248=CONTEXT_DEPENDENT_SHAPE_REPRESENTATION(#173,#10243);
#249=CONTEXT_DEPENDENT_SHAPE_REPRESENTATION(#174,#10244);
#250=CONTEXT_DEPENDENT_SHAPE_REPRESENTATION(#175,#10245);
#251=CONTEXT_DEPENDENT_SHAPE_REPRESENTATION(#176,#10246);
#252=NEXT_ASSEMBLY_USAGE_OCCURRENCE('Body inlet half:2',
'Body inlet half:2','Body inlet half:2',#10286,#10287,
'Body inlet half:2');
#253=NEXT_ASSEMBLY_USAGE_OCCURRENCE('Body outlet half:2',
'Body outlet half:2','Body outlet half:2',#10286,#10288,
'Body outlet half:2');
#254=NEXT_ASSEMBLY_USAGE_OCCURRENCE('Split-body gasket:2',
'Split-body gasket:2','Split-body gasket:2',#10286,#10289,
'Split-body gasket:2');
#255=NEXT_ASSEMBLY_USAGE_OCCURRENCE('Stem guide:2','Stem guide:2',
'Stem guide:2',#10286,#10290,'Stem guide:2');
#256=NEXT_ASSEMBLY_USAGE_OCCURRENCE('Packing ring:2','Packing ring:2',
'Packing ring:2',#10286,#10291,'Packing ring:2');
#257=NEXT_ASSEMBLY_USAGE_OCCURRENCE('Packing retainer:2',
'Packing retainer:2','Packing retainer:2',#10286,#10292,
'Packing retainer:2');
#258=NEXT_ASSEMBLY_USAGE_OCCURRENCE('Lever stop bridge:2',
'Lever stop bridge:2','Lever stop bridge:2',#10286,#10293,
'Lever stop bridge:2');
#259=NEXT_ASSEMBLY_USAGE_OCCURRENCE('Ball seat:2','Ball seat:2',
'Ball seat:2',#10286,#10294,'Ball seat:2');
#260=NEXT_ASSEMBLY_USAGE_OCCURRENCE('Ball seat:3','Ball seat:3',
'Ball seat:3',#10286,#10294,'Ball seat:3');
#261=NEXT_ASSEMBLY_USAGE_OCCURRENCE('Flat Washer - M5:2',
'Flat Washer - M5:2','Flat Washer - M5:2',#10286,#10296,
'Flat Washer - M5:2');
#262=NEXT_ASSEMBLY_USAGE_OCCURRENCE('M5x70 body screw:2',
'M5x70 body screw:2','M5x70 body screw:2',#10286,#10295,
'M5x70 body screw:2');
#263=NEXT_ASSEMBLY_USAGE_OCCURRENCE('Flat Washer - M5:3',
'Flat Washer - M5:3','Flat Washer - M5:3',#10286,#10296,
'Flat Washer - M5:3');
#264=NEXT_ASSEMBLY_USAGE_OCCURRENCE('Hex Nut - M5:2','Hex Nut - M5:2',
'Hex Nut - M5:2',#10286,#10297,'Hex Nut - M5:2');
#265=NEXT_ASSEMBLY_USAGE_OCCURRENCE('Flat Washer - M5:4',
'Flat Washer - M5:4','Flat Washer - M5:4',#10286,#10296,
'Flat Washer - M5:4');
#266=NEXT_ASSEMBLY_USAGE_OCCURRENCE('M5x70 body screw:3',
'M5x70 body screw:3','M5x70 body screw:3',#10286,#10295,
'M5x70 body screw:3');
#267=NEXT_ASSEMBLY_USAGE_OCCURRENCE('Flat Washer - M5:5',
'Flat Washer - M5:5','Flat Washer - M5:5',#10286,#10296,
'Flat Washer - M5:5');
#268=NEXT_ASSEMBLY_USAGE_OCCURRENCE('Hex Nut - M5:3','Hex Nut - M5:3',
'Hex Nut - M5:3',#10286,#10297,'Hex Nut - M5:3');
#269=NEXT_ASSEMBLY_USAGE_OCCURRENCE('Flat Washer - M5:6',
'Flat Washer - M5:6','Flat Washer - M5:6',#10286,#10296,
'Flat Washer - M5:6');
#270=NEXT_ASSEMBLY_USAGE_OCCURRENCE('M5x70 body screw:4',
'M5x70 body screw:4','M5x70 body screw:4',#10286,#10295,
'M5x70 body screw:4');
#271=NEXT_ASSEMBLY_USAGE_OCCURRENCE('Flat Washer - M5:7',
'Flat Washer - M5:7','Flat Washer - M5:7',#10286,#10296,
'Flat Washer - M5:7');
#272=NEXT_ASSEMBLY_USAGE_OCCURRENCE('Hex Nut - M5:4','Hex Nut - M5:4',
'Hex Nut - M5:4',#10286,#10297,'Hex Nut - M5:4');
#273=NEXT_ASSEMBLY_USAGE_OCCURRENCE('Flat Washer - M5:8',
'Flat Washer - M5:8','Flat Washer - M5:8',#10286,#10296,
'Flat Washer - M5:8');
#274=NEXT_ASSEMBLY_USAGE_OCCURRENCE('M5x70 body screw:5',
'M5x70 body screw:5','M5x70 body screw:5',#10286,#10295,
'M5x70 body screw:5');
#275=NEXT_ASSEMBLY_USAGE_OCCURRENCE('Flat Washer - M5:9',
'Flat Washer - M5:9','Flat Washer - M5:9',#10286,#10296,
'Flat Washer - M5:9');
#276=NEXT_ASSEMBLY_USAGE_OCCURRENCE('Hex Nut - M5:5','Hex Nut - M5:5',
'Hex Nut - M5:5',#10286,#10297,'Hex Nut - M5:5');
#277=NEXT_ASSEMBLY_USAGE_OCCURRENCE('Bridge spacer:2','Bridge spacer:2',
'Bridge spacer:2',#10286,#10298,'Bridge spacer:2');
#278=NEXT_ASSEMBLY_USAGE_OCCURRENCE('Cap Screw - M4x16:2',
'Cap Screw - M4x16:2','Cap Screw - M4x16:2',#10286,#10299,
'Cap Screw - M4x16:2');
#279=NEXT_ASSEMBLY_USAGE_OCCURRENCE('Bridge spacer:3','Bridge spacer:3',
'Bridge spacer:3',#10286,#10298,'Bridge spacer:3');
#280=NEXT_ASSEMBLY_USAGE_OCCURRENCE('Cap Screw - M4x16:3',
'Cap Screw - M4x16:3','Cap Screw - M4x16:3',#10286,#10299,
'Cap Screw - M4x16:3');
#281=NEXT_ASSEMBLY_USAGE_OCCURRENCE('Bridge spacer:4','Bridge spacer:4',
'Bridge spacer:4',#10286,#10298,'Bridge spacer:4');
#282=NEXT_ASSEMBLY_USAGE_OCCURRENCE('Cap Screw - M4x16:4',
'Cap Screw - M4x16:4','Cap Screw - M4x16:4',#10286,#10299,
'Cap Screw - M4x16:4');
#283=NEXT_ASSEMBLY_USAGE_OCCURRENCE('Bridge spacer:5','Bridge spacer:5',
'Bridge spacer:5',#10286,#10298,'Bridge spacer:5');
#284=NEXT_ASSEMBLY_USAGE_OCCURRENCE('Cap Screw - M4x16:5',
'Cap Screw - M4x16:5','Cap Screw - M4x16:5',#10286,#10299,
'Cap Screw - M4x16:5');
#285=NEXT_ASSEMBLY_USAGE_OCCURRENCE('Stop pin:2','Stop pin:2',
'Stop pin:2',#10286,#10300,'Stop pin:2');
#286=NEXT_ASSEMBLY_USAGE_OCCURRENCE('Stop pin:3','Stop pin:3',
'Stop pin:3',#10286,#10300,'Stop pin:3');
#287=NEXT_ASSEMBLY_USAGE_OCCURRENCE('Bypass valve body:1',
'Bypass valve body:1','Bypass valve body:1',#10285,#10286,
'Bypass valve body:1');
#288=NEXT_ASSEMBLY_USAGE_OCCURRENCE('Union gasket:2','Union gasket:2',
'Union gasket:2',#10285,#10301,'Union gasket:2');
#289=NEXT_ASSEMBLY_USAGE_OCCURRENCE('Bypass tee:1','Bypass tee:1',
'Bypass tee:1',#10285,#10302,'Bypass tee:1');
#290=NEXT_ASSEMBLY_USAGE_OCCURRENCE('Main-run pipe:1','Main-run pipe:1',
'Main-run pipe:1',#10285,#10303,'Main-run pipe:1');
#291=NEXT_ASSEMBLY_USAGE_OCCURRENCE('Bypass side pipe:1',
'Bypass side pipe:1','Bypass side pipe:1',#10285,#10304,
'Bypass side pipe:1');
#292=NEXT_ASSEMBLY_USAGE_OCCURRENCE('Bypass valve pipe:1',
'Bypass valve pipe:1','Bypass valve pipe:1',#10285,#10305,
'Bypass valve pipe:1');
#293=NEXT_ASSEMBLY_USAGE_OCCURRENCE('Bypass tee:2','Bypass tee:2',
'Bypass tee:2',#10285,#10302,'Bypass tee:2');
#294=NEXT_ASSEMBLY_USAGE_OCCURRENCE('Main-run pipe:2','Main-run pipe:2',
'Main-run pipe:2',#10285,#10303,'Main-run pipe:2');
#295=NEXT_ASSEMBLY_USAGE_OCCURRENCE('Bypass side pipe:2',
'Bypass side pipe:2','Bypass side pipe:2',#10285,#10304,
'Bypass side pipe:2');
#296=NEXT_ASSEMBLY_USAGE_OCCURRENCE('Bypass valve pipe:2',
'Bypass valve pipe:2','Bypass valve pipe:2',#10285,#10305,
'Bypass valve pipe:2');
#297=NEXT_ASSEMBLY_USAGE_OCCURRENCE(
'Pipe Elbow - 90 Degrees, 1-2 Inch Tapered Pipe Thread:2',
'Pipe Elbow - 90 Degrees, 1-2 Inch Tapered Pipe Thread:2',
'Pipe Elbow - 90 Degrees, 1-2 Inch Tapered Pipe Thread:2',#10285,#10306,
'Pipe Elbow - 90 Degrees, 1-2 Inch Tapered Pipe Thread:2');
#298=NEXT_ASSEMBLY_USAGE_OCCURRENCE(
'Pipe Elbow - 90 Degrees, 1-2 Inch Tapered Pipe Thread:3',
'Pipe Elbow - 90 Degrees, 1-2 Inch Tapered Pipe Thread:3',
'Pipe Elbow - 90 Degrees, 1-2 Inch Tapered Pipe Thread:3',#10285,#10306,
'Pipe Elbow - 90 Degrees, 1-2 Inch Tapered Pipe Thread:3');
#299=NEXT_ASSEMBLY_USAGE_OCCURRENCE(
'Hex Pipe Nipple - 1-2 Inch Tapered Pipe Thread:4',
'Hex Pipe Nipple - 1-2 Inch Tapered Pipe Thread:4',
'Hex Pipe Nipple - 1-2 Inch Tapered Pipe Thread:4',#10285,#10307,
'Hex Pipe Nipple - 1-2 Inch Tapered Pipe Thread:4');
#300=NEXT_ASSEMBLY_USAGE_OCCURRENCE(
'Hex Pipe Nipple - 1-2 Inch Tapered Pipe Thread:5',
'Hex Pipe Nipple - 1-2 Inch Tapered Pipe Thread:5',
'Hex Pipe Nipple - 1-2 Inch Tapered Pipe Thread:5',#10285,#10307,
'Hex Pipe Nipple - 1-2 Inch Tapered Pipe Thread:5');
#301=NEXT_ASSEMBLY_USAGE_OCCURRENCE('Union half A:2','Union half A:2',
'Union half A:2',#10285,#10308,'Union half A:2');
#302=NEXT_ASSEMBLY_USAGE_OCCURRENCE('Union half B:2','Union half B:2',
'Union half B:2',#10285,#10309,'Union half B:2');
#303=NEXT_ASSEMBLY_USAGE_OCCURRENCE('Flat Washer - M8:2',
'Flat Washer - M8:2','Flat Washer - M8:2',#10285,#10311,
'Flat Washer - M8:2');
#304=NEXT_ASSEMBLY_USAGE_OCCURRENCE('Cap Screw - M8x30:2',
'Cap Screw - M8x30:2','Cap Screw - M8x30:2',#10285,#10310,
'Cap Screw - M8x30:2');
#305=NEXT_ASSEMBLY_USAGE_OCCURRENCE('Flat Washer - M8:3',
'Flat Washer - M8:3','Flat Washer - M8:3',#10285,#10311,
'Flat Washer - M8:3');
#306=NEXT_ASSEMBLY_USAGE_OCCURRENCE('Hex Nut - M8:2','Hex Nut - M8:2',
'Hex Nut - M8:2',#10285,#10312,'Hex Nut - M8:2');
#307=NEXT_ASSEMBLY_USAGE_OCCURRENCE('Flat Washer - M8:4',
'Flat Washer - M8:4','Flat Washer - M8:4',#10285,#10311,
'Flat Washer - M8:4');
#308=NEXT_ASSEMBLY_USAGE_OCCURRENCE('Cap Screw - M8x30:3',
'Cap Screw - M8x30:3','Cap Screw - M8x30:3',#10285,#10310,
'Cap Screw - M8x30:3');
#309=NEXT_ASSEMBLY_USAGE_OCCURRENCE('Flat Washer - M8:5',
'Flat Washer - M8:5','Flat Washer - M8:5',#10285,#10311,
'Flat Washer - M8:5');
#310=NEXT_ASSEMBLY_USAGE_OCCURRENCE('Hex Nut - M8:3','Hex Nut - M8:3',
'Hex Nut - M8:3',#10285,#10312,'Hex Nut - M8:3');
#311=NEXT_ASSEMBLY_USAGE_OCCURRENCE('Flat Washer - M8:6',
'Flat Washer - M8:6','Flat Washer - M8:6',#10285,#10311,
'Flat Washer - M8:6');
#312=NEXT_ASSEMBLY_USAGE_OCCURRENCE('Cap Screw - M8x30:4',
'Cap Screw - M8x30:4','Cap Screw - M8x30:4',#10285,#10310,
'Cap Screw - M8x30:4');
#313=NEXT_ASSEMBLY_USAGE_OCCURRENCE('Flat Washer - M8:7',
'Flat Washer - M8:7','Flat Washer - M8:7',#10285,#10311,
'Flat Washer - M8:7');
#314=NEXT_ASSEMBLY_USAGE_OCCURRENCE('Hex Nut - M8:4','Hex Nut - M8:4',
'Hex Nut - M8:4',#10285,#10312,'Hex Nut - M8:4');
#315=NEXT_ASSEMBLY_USAGE_OCCURRENCE('Flat Washer - M8:8',
'Flat Washer - M8:8','Flat Washer - M8:8',#10285,#10311,
'Flat Washer - M8:8');
#316=NEXT_ASSEMBLY_USAGE_OCCURRENCE('Cap Screw - M8x30:5',
'Cap Screw - M8x30:5','Cap Screw - M8x30:5',#10285,#10310,
'Cap Screw - M8x30:5');
#317=NEXT_ASSEMBLY_USAGE_OCCURRENCE('Flat Washer - M8:9',
'Flat Washer - M8:9','Flat Washer - M8:9',#10285,#10311,
'Flat Washer - M8:9');
#318=NEXT_ASSEMBLY_USAGE_OCCURRENCE('Hex Nut - M8:5','Hex Nut - M8:5',
'Hex Nut - M8:5',#10285,#10312,'Hex Nut - M8:5');
#319=NEXT_ASSEMBLY_USAGE_OCCURRENCE('Ported ball:2','Ported ball:2',
'Ported ball:2',#10313,#10314,'Ported ball:2');
#320=NEXT_ASSEMBLY_USAGE_OCCURRENCE('Stem:2','Stem:2','Stem:2',#10313,#10315,
'Stem:2');
#321=NEXT_ASSEMBLY_USAGE_OCCURRENCE('Lever:2','Lever:2','Lever:2',#10313,
#10316,'Lever:2');
#322=NEXT_ASSEMBLY_USAGE_OCCURRENCE('Lever keeper:2','Lever keeper:2',
'Lever keeper:2',#10313,#10317,'Lever keeper:2');
#323=NEXT_ASSEMBLY_USAGE_OCCURRENCE('Bonded grip:2','Bonded grip:2',
'Bonded grip:2',#10313,#10318,'Bonded grip:2');
#324=NEXT_ASSEMBLY_USAGE_OCCURRENCE('M4x10 Cap Screw:2',
'M4x10 Cap Screw:2','M4x10 Cap Screw:2',#10313,#10319,
'M4x10 Cap Screw:2');
#325=NEXT_ASSEMBLY_USAGE_OCCURRENCE('Pipe loop union and valve body:1',
'Pipe loop union and valve body:1','Pipe loop union and valve body:1',#10284,
#10285,'Pipe loop union and valve body:1');
#326=NEXT_ASSEMBLY_USAGE_OCCURRENCE('Bypass valve rotor:1',
'Bypass valve rotor:1','Bypass valve rotor:1',#10284,#10313,
'Bypass valve rotor:1');
#327=(
BOUNDED_CURVE()
B_SPLINE_CURVE(2,(#8945,#8946,#8947),.UNSPECIFIED.,.F.,.F.)
B_SPLINE_CURVE_WITH_KNOTS((3,3),(0.140651836354967,0.670383167684795),
 .UNSPECIFIED.)
CURVE()
GEOMETRIC_REPRESENTATION_ITEM()
RATIONAL_B_SPLINE_CURVE((1.11602540378444,1.28867513459481,1.11602540378444))
REPRESENTATION_ITEM('')
);
#328=(
BOUNDED_CURVE()
B_SPLINE_CURVE(2,(#8949,#8950,#8951),.UNSPECIFIED.,.F.,.F.)
B_SPLINE_CURVE_WITH_KNOTS((3,3),(0.140651836354967,0.670383167684795),
 .UNSPECIFIED.)
CURVE()
GEOMETRIC_REPRESENTATION_ITEM()
RATIONAL_B_SPLINE_CURVE((1.11602540378444,1.28867513459481,1.11602540378444))
REPRESENTATION_ITEM('')
);
#329=(
BOUNDED_CURVE()
B_SPLINE_CURVE(2,(#8956,#8957,#8958),.UNSPECIFIED.,.F.,.F.)
B_SPLINE_CURVE_WITH_KNOTS((3,3),(0.140651836354967,0.670383167684795),
 .UNSPECIFIED.)
CURVE()
GEOMETRIC_REPRESENTATION_ITEM()
RATIONAL_B_SPLINE_CURVE((1.11602540378444,1.28867513459481,1.11602540378444))
REPRESENTATION_ITEM('')
);
#330=(
BOUNDED_CURVE()
B_SPLINE_CURVE(2,(#8960,#8961,#8962),.UNSPECIFIED.,.F.,.F.)
B_SPLINE_CURVE_WITH_KNOTS((3,3),(0.140651836354967,0.670383167684795),
 .UNSPECIFIED.)
CURVE()
GEOMETRIC_REPRESENTATION_ITEM()
RATIONAL_B_SPLINE_CURVE((1.11602540378444,1.28867513459481,1.11602540378444))
REPRESENTATION_ITEM('')
);
#331=(
BOUNDED_CURVE()
B_SPLINE_CURVE(2,(#8964,#8965,#8966),.UNSPECIFIED.,.F.,.F.)
B_SPLINE_CURVE_WITH_KNOTS((3,3),(0.140651836354967,0.670383167684795),
 .UNSPECIFIED.)
CURVE()
GEOMETRIC_REPRESENTATION_ITEM()
RATIONAL_B_SPLINE_CURVE((1.11602540378444,1.28867513459481,1.11602540378444))
REPRESENTATION_ITEM('')
);
#332=(
BOUNDED_CURVE()
B_SPLINE_CURVE(2,(#8967,#8968,#8969),.UNSPECIFIED.,.F.,.F.)
B_SPLINE_CURVE_WITH_KNOTS((3,3),(0.140651836354967,0.670383167684795),
 .UNSPECIFIED.)
CURVE()
GEOMETRIC_REPRESENTATION_ITEM()
RATIONAL_B_SPLINE_CURVE((1.11602540378444,1.28867513459481,1.11602540378444))
REPRESENTATION_ITEM('')
);
#333=(
BOUNDED_CURVE()
B_SPLINE_CURVE(2,(#8976,#8977,#8978),.UNSPECIFIED.,.F.,.F.)
B_SPLINE_CURVE_WITH_KNOTS((3,3),(0.140651836354967,0.670383167684795),
 .UNSPECIFIED.)
CURVE()
GEOMETRIC_REPRESENTATION_ITEM()
RATIONAL_B_SPLINE_CURVE((1.11602540378444,1.28867513459481,1.11602540378444))
REPRESENTATION_ITEM('')
);
#334=(
BOUNDED_CURVE()
B_SPLINE_CURVE(2,(#8980,#8981,#8982),.UNSPECIFIED.,.F.,.F.)
B_SPLINE_CURVE_WITH_KNOTS((3,3),(0.140651836354967,0.670383167684796),
 .UNSPECIFIED.)
CURVE()
GEOMETRIC_REPRESENTATION_ITEM()
RATIONAL_B_SPLINE_CURVE((1.11602540378444,1.28867513459481,1.11602540378444))
REPRESENTATION_ITEM('')
);
#335=(
BOUNDED_CURVE()
B_SPLINE_CURVE(2,(#8984,#8985,#8986),.UNSPECIFIED.,.F.,.F.)
B_SPLINE_CURVE_WITH_KNOTS((3,3),(0.140651836354967,0.670383167684795),
 .UNSPECIFIED.)
CURVE()
GEOMETRIC_REPRESENTATION_ITEM()
RATIONAL_B_SPLINE_CURVE((1.11602540378444,1.28867513459481,1.11602540378444))
REPRESENTATION_ITEM('')
);
#336=(
BOUNDED_CURVE()
B_SPLINE_CURVE(2,(#8988,#8989,#8990),.UNSPECIFIED.,.F.,.F.)
B_SPLINE_CURVE_WITH_KNOTS((3,3),(0.140651836354967,0.670383167684795),
 .UNSPECIFIED.)
CURVE()
GEOMETRIC_REPRESENTATION_ITEM()
RATIONAL_B_SPLINE_CURVE((1.11602540378444,1.28867513459482,1.11602540378444))
REPRESENTATION_ITEM('')
);
#337=(
BOUNDED_CURVE()
B_SPLINE_CURVE(2,(#8992,#8993,#8994),.UNSPECIFIED.,.F.,.F.)
B_SPLINE_CURVE_WITH_KNOTS((3,3),(0.140651836354967,0.670383167684795),
 .UNSPECIFIED.)
CURVE()
GEOMETRIC_REPRESENTATION_ITEM()
RATIONAL_B_SPLINE_CURVE((1.11602540378444,1.28867513459481,1.11602540378444))
REPRESENTATION_ITEM('')
);
#338=(
BOUNDED_CURVE()
B_SPLINE_CURVE(2,(#8995,#8996,#8997),.UNSPECIFIED.,.F.,.F.)
B_SPLINE_CURVE_WITH_KNOTS((3,3),(0.140651836354967,0.670383167684795),
 .UNSPECIFIED.)
CURVE()
GEOMETRIC_REPRESENTATION_ITEM()
RATIONAL_B_SPLINE_CURVE((1.11602540378444,1.28867513459481,1.11602540378444))
REPRESENTATION_ITEM('')
);
#339=(
BOUNDED_CURVE()
B_SPLINE_CURVE(2,(#9615,#9616,#9617),.UNSPECIFIED.,.F.,.F.)
B_SPLINE_CURVE_WITH_KNOTS((3,3),(0.14973948338295,0.97160236658079),
 .UNSPECIFIED.)
CURVE()
GEOMETRIC_REPRESENTATION_ITEM()
RATIONAL_B_SPLINE_CURVE((1.07140024848292,1.23714644374248,1.07140024848292))
REPRESENTATION_ITEM('')
);
#340=(
BOUNDED_CURVE()
B_SPLINE_CURVE(2,(#9619,#9620,#9621),.UNSPECIFIED.,.F.,.F.)
B_SPLINE_CURVE_WITH_KNOTS((3,3),(0.14973948338295,0.971602366580789),
 .UNSPECIFIED.)
CURVE()
GEOMETRIC_REPRESENTATION_ITEM()
RATIONAL_B_SPLINE_CURVE((1.07140024848292,1.23714644374248,1.07140024848292))
REPRESENTATION_ITEM('')
);
#341=(
BOUNDED_CURVE()
B_SPLINE_CURVE(2,(#9626,#9627,#9628),.UNSPECIFIED.,.F.,.F.)
B_SPLINE_CURVE_WITH_KNOTS((3,3),(0.14973948338295,0.97160236658079),
 .UNSPECIFIED.)
CURVE()
GEOMETRIC_REPRESENTATION_ITEM()
RATIONAL_B_SPLINE_CURVE((1.07140024848292,1.23714644374248,1.07140024848292))
REPRESENTATION_ITEM('')
);
#342=(
BOUNDED_CURVE()
B_SPLINE_CURVE(2,(#9630,#9631,#9632),.UNSPECIFIED.,.F.,.F.)
B_SPLINE_CURVE_WITH_KNOTS((3,3),(0.14973948338295,0.97160236658079),
 .UNSPECIFIED.)
CURVE()
GEOMETRIC_REPRESENTATION_ITEM()
RATIONAL_B_SPLINE_CURVE((1.07140024848292,1.23714644374248,1.07140024848292))
REPRESENTATION_ITEM('')
);
#343=(
BOUNDED_CURVE()
B_SPLINE_CURVE(2,(#9634,#9635,#9636),.UNSPECIFIED.,.F.,.F.)
B_SPLINE_CURVE_WITH_KNOTS((3,3),(0.14973948338295,0.971602366580789),
 .UNSPECIFIED.)
CURVE()
GEOMETRIC_REPRESENTATION_ITEM()
RATIONAL_B_SPLINE_CURVE((1.07140024848292,1.23714644374248,1.07140024848292))
REPRESENTATION_ITEM('')
);
#344=(
BOUNDED_CURVE()
B_SPLINE_CURVE(2,(#9637,#9638,#9639),.UNSPECIFIED.,.F.,.F.)
B_SPLINE_CURVE_WITH_KNOTS((3,3),(0.14973948338295,0.97160236658079),
 .UNSPECIFIED.)
CURVE()
GEOMETRIC_REPRESENTATION_ITEM()
RATIONAL_B_SPLINE_CURVE((1.07140024848292,1.23714644374248,1.07140024848292))
REPRESENTATION_ITEM('')
);
#345=(
BOUNDED_CURVE()
B_SPLINE_CURVE(2,(#9646,#9647,#9648),.UNSPECIFIED.,.F.,.F.)
B_SPLINE_CURVE_WITH_KNOTS((3,3),(0.14973948338295,0.97160236658079),
 .UNSPECIFIED.)
CURVE()
GEOMETRIC_REPRESENTATION_ITEM()
RATIONAL_B_SPLINE_CURVE((1.07140024848292,1.23714644374248,1.07140024848292))
REPRESENTATION_ITEM('')
);
#346=(
BOUNDED_CURVE()
B_SPLINE_CURVE(2,(#9650,#9651,#9652),.UNSPECIFIED.,.F.,.F.)
B_SPLINE_CURVE_WITH_KNOTS((3,3),(0.14973948338295,0.97160236658079),
 .UNSPECIFIED.)
CURVE()
GEOMETRIC_REPRESENTATION_ITEM()
RATIONAL_B_SPLINE_CURVE((1.07140024848292,1.23714644374248,1.07140024848292))
REPRESENTATION_ITEM('')
);
#347=(
BOUNDED_CURVE()
B_SPLINE_CURVE(2,(#9654,#9655,#9656),.UNSPECIFIED.,.F.,.F.)
B_SPLINE_CURVE_WITH_KNOTS((3,3),(0.14973948338295,0.971602366580789),
 .UNSPECIFIED.)
CURVE()
GEOMETRIC_REPRESENTATION_ITEM()
RATIONAL_B_SPLINE_CURVE((1.07140024848292,1.23714644374248,1.07140024848292))
REPRESENTATION_ITEM('')
);
#348=(
BOUNDED_CURVE()
B_SPLINE_CURVE(2,(#9658,#9659,#9660),.UNSPECIFIED.,.F.,.F.)
B_SPLINE_CURVE_WITH_KNOTS((3,3),(0.14973948338295,0.97160236658079),
 .UNSPECIFIED.)
CURVE()
GEOMETRIC_REPRESENTATION_ITEM()
RATIONAL_B_SPLINE_CURVE((1.07140024848292,1.23714644374248,1.07140024848292))
REPRESENTATION_ITEM('')
);
#349=(
BOUNDED_CURVE()
B_SPLINE_CURVE(2,(#9662,#9663,#9664),.UNSPECIFIED.,.F.,.F.)
B_SPLINE_CURVE_WITH_KNOTS((3,3),(0.14973948338295,0.97160236658079),
 .UNSPECIFIED.)
CURVE()
GEOMETRIC_REPRESENTATION_ITEM()
RATIONAL_B_SPLINE_CURVE((1.07140024848292,1.23714644374248,1.07140024848292))
REPRESENTATION_ITEM('')
);
#350=(
BOUNDED_CURVE()
B_SPLINE_CURVE(2,(#9665,#9666,#9667),.UNSPECIFIED.,.F.,.F.)
B_SPLINE_CURVE_WITH_KNOTS((3,3),(0.14973948338295,0.971602366580789),
 .UNSPECIFIED.)
CURVE()
GEOMETRIC_REPRESENTATION_ITEM()
RATIONAL_B_SPLINE_CURVE((1.07140024848292,1.23714644374248,1.07140024848292))
REPRESENTATION_ITEM('')
);
#351=CONICAL_SURFACE('',#6109,0.4,0.785398163397448);
#352=CONICAL_SURFACE('',#6113,0.41,0.785398163397448);
#353=CONICAL_SURFACE('',#6117,0.26,0.463647609000806);
#354=CONICAL_SURFACE('',#6121,0.275,0.785398163397449);
#355=CONICAL_SURFACE('',#6132,0.47094010767585,1.0471975511966);
#356=CONICAL_SURFACE('',#6134,0.47094010767585,1.0471975511966);
#357=CONICAL_SURFACE('',#6159,0.325,0.785398163397448);
#358=CONICAL_SURFACE('',#6163,0.335,0.785398163397448);
#359=CONICAL_SURFACE('',#6167,0.21,0.463647609000806);
#360=CONICAL_SURFACE('',#6171,0.18,0.785398163397448);
#361=CONICAL_SURFACE('',#6367,1.025,0.785398163397448);
#362=CONICAL_SURFACE('',#6370,1.025,0.785398163397448);
#363=CONICAL_SURFACE('',#6428,0.625,0.785398163397448);
#364=CONICAL_SURFACE('',#6432,0.635,0.785398163397449);
#365=CONICAL_SURFACE('',#6436,0.41,0.463647609000806);
#366=CONICAL_SURFACE('',#6440,0.36,0.785398163397448);
#367=CONICAL_SURFACE('',#6461,0.734027674973257,1.0471975511966);
#368=CONICAL_SURFACE('',#6463,0.734027674973257,1.0471975511966);
#369=CONICAL_SURFACE('',#6600,0.325,0.785398163397448);
#370=CONICAL_SURFACE('',#6604,0.335,0.785398163397448);
#371=CONICAL_SURFACE('',#6608,0.21,0.463647609000806);
#372=ORIENTED_CLOSED_SHELL('',*,#5524,.F.);
#373=ORIENTED_CLOSED_SHELL('',*,#5530,.F.);
#374=ORIENTED_CLOSED_SHELL('',*,#5542,.F.);
#375=ORIENTED_CLOSED_SHELL('',*,#5550,.F.);
#376=BREP_WITH_VOIDS('Body1',#5525,(#372));
#377=BREP_WITH_VOIDS('Body1',#5529,(#373));
#378=BREP_WITH_VOIDS('Body1',#5541,(#374));
#379=BREP_WITH_VOIDS('Body1',#5551,(#375));
#380=TOROIDAL_SURFACE('',#6035,0.5,0.1);
#381=SHAPE_REPRESENTATION_RELATIONSHIP('SRR','None',#10250,#413);
#382=SHAPE_REPRESENTATION_RELATIONSHIP('SRR','None',#10251,#414);
#383=SHAPE_REPRESENTATION_RELATIONSHIP('SRR','None',#10252,#415);
#384=SHAPE_REPRESENTATION_RELATIONSHIP('SRR','None',#10253,#416);
#385=SHAPE_REPRESENTATION_RELATIONSHIP('SRR','None',#10254,#417);
#386=SHAPE_REPRESENTATION_RELATIONSHIP('SRR','None',#10255,#418);
#387=SHAPE_REPRESENTATION_RELATIONSHIP('SRR','None',#10256,#419);
#388=SHAPE_REPRESENTATION_RELATIONSHIP('SRR','None',#10257,#420);
#389=SHAPE_REPRESENTATION_RELATIONSHIP('SRR','None',#10258,#421);
#390=SHAPE_REPRESENTATION_RELATIONSHIP('SRR','None',#10259,#422);
#391=SHAPE_REPRESENTATION_RELATIONSHIP('SRR','None',#10260,#423);
#392=SHAPE_REPRESENTATION_RELATIONSHIP('SRR','None',#10261,#424);
#393=SHAPE_REPRESENTATION_RELATIONSHIP('SRR','None',#10262,#425);
#394=SHAPE_REPRESENTATION_RELATIONSHIP('SRR','None',#10263,#426);
#395=SHAPE_REPRESENTATION_RELATIONSHIP('SRR','None',#10264,#427);
#396=SHAPE_REPRESENTATION_RELATIONSHIP('SRR','None',#10265,#428);
#397=SHAPE_REPRESENTATION_RELATIONSHIP('SRR','None',#10266,#429);
#398=SHAPE_REPRESENTATION_RELATIONSHIP('SRR','None',#10267,#430);
#399=SHAPE_REPRESENTATION_RELATIONSHIP('SRR','None',#10268,#431);
#400=SHAPE_REPRESENTATION_RELATIONSHIP('SRR','None',#10269,#432);
#401=SHAPE_REPRESENTATION_RELATIONSHIP('SRR','None',#10270,#433);
#402=SHAPE_REPRESENTATION_RELATIONSHIP('SRR','None',#10271,#434);
#403=SHAPE_REPRESENTATION_RELATIONSHIP('SRR','None',#10272,#435);
#404=SHAPE_REPRESENTATION_RELATIONSHIP('SRR','None',#10273,#436);
#405=SHAPE_REPRESENTATION_RELATIONSHIP('SRR','None',#10274,#437);
#406=SHAPE_REPRESENTATION_RELATIONSHIP('SRR','None',#10275,#438);
#407=SHAPE_REPRESENTATION_RELATIONSHIP('SRR','None',#10277,#439);
#408=SHAPE_REPRESENTATION_RELATIONSHIP('SRR','None',#10278,#440);
#409=SHAPE_REPRESENTATION_RELATIONSHIP('SRR','None',#10279,#441);
#410=SHAPE_REPRESENTATION_RELATIONSHIP('SRR','None',#10280,#442);
#411=SHAPE_REPRESENTATION_RELATIONSHIP('SRR','None',#10281,#443);
#412=SHAPE_REPRESENTATION_RELATIONSHIP('SRR','None',#10282,#444);
#413=ADVANCED_BREP_SHAPE_REPRESENTATION('',(#477),#10062);
#414=ADVANCED_BREP_SHAPE_REPRESENTATION('',(#478),#10063);
#415=ADVANCED_BREP_SHAPE_REPRESENTATION('',(#479),#10064);
#416=ADVANCED_BREP_SHAPE_REPRESENTATION('',(#480),#10065);
#417=ADVANCED_BREP_SHAPE_REPRESENTATION('',(#481),#10066);
#418=ADVANCED_BREP_SHAPE_REPRESENTATION('',(#482),#10067);
#419=ADVANCED_BREP_SHAPE_REPRESENTATION('',(#483),#10068);
#420=ADVANCED_BREP_SHAPE_REPRESENTATION('',(#484),#10069);
#421=ADVANCED_BREP_SHAPE_REPRESENTATION('',(#376),#10070);
#422=ADVANCED_BREP_SHAPE_REPRESENTATION('',(#485),#10071);
#423=ADVANCED_BREP_SHAPE_REPRESENTATION('',(#486),#10072);
#424=ADVANCED_BREP_SHAPE_REPRESENTATION('',(#487),#10073);
#425=ADVANCED_BREP_SHAPE_REPRESENTATION('',(#377),#10074);
#426=ADVANCED_BREP_SHAPE_REPRESENTATION('',(#488),#10075);
#427=ADVANCED_BREP_SHAPE_REPRESENTATION('',(#489),#10076);
#428=ADVANCED_BREP_SHAPE_REPRESENTATION('',(#490),#10077);
#429=ADVANCED_BREP_SHAPE_REPRESENTATION('',(#491),#10078);
#430=ADVANCED_BREP_SHAPE_REPRESENTATION('',(#492),#10079);
#431=ADVANCED_BREP_SHAPE_REPRESENTATION('',(#493),#10080);
#432=ADVANCED_BREP_SHAPE_REPRESENTATION('',(#494),#10081);
#433=ADVANCED_BREP_SHAPE_REPRESENTATION('',(#495),#10082);
#434=ADVANCED_BREP_SHAPE_REPRESENTATION('',(#496),#10083);
#435=ADVANCED_BREP_SHAPE_REPRESENTATION('',(#497),#10084);
#436=ADVANCED_BREP_SHAPE_REPRESENTATION('',(#378),#10085);
#437=ADVANCED_BREP_SHAPE_REPRESENTATION('',(#498),#10086);
#438=ADVANCED_BREP_SHAPE_REPRESENTATION('',(#499),#10087);
#439=ADVANCED_BREP_SHAPE_REPRESENTATION('',(#500),#10089);
#440=ADVANCED_BREP_SHAPE_REPRESENTATION('',(#501),#10090);
#441=ADVANCED_BREP_SHAPE_REPRESENTATION('',(#502),#10091);
#442=ADVANCED_BREP_SHAPE_REPRESENTATION('',(#503),#10092);
#443=ADVANCED_BREP_SHAPE_REPRESENTATION('',(#504),#10093);
#444=ADVANCED_BREP_SHAPE_REPRESENTATION('',(#379),#10094);
#445=STYLED_ITEM('',(#10479),#477);
#446=STYLED_ITEM('',(#10479),#478);
#447=STYLED_ITEM('',(#10479),#479);
#448=STYLED_ITEM('',(#10493),#480);
#449=STYLED_ITEM('',(#10493),#481);
#450=STYLED_ITEM('',(#10486),#482);
#451=STYLED_ITEM('',(#10486),#483);
#452=STYLED_ITEM('',(#10486),#484);
#453=STYLED_ITEM('',(#10507),#376);
#454=STYLED_ITEM('',(#10507),#485);
#455=STYLED_ITEM('',(#10507),#486);
#456=STYLED_ITEM('',(#10493),#487);
#457=STYLED_ITEM('',(#10507),#377);
#458=STYLED_ITEM('',(#10500),#488);
#459=STYLED_ITEM('',(#10486),#489);
#460=STYLED_ITEM('',(#10493),#490);
#461=STYLED_ITEM('',(#10486),#491);
#462=STYLED_ITEM('',(#10493),#492);
#463=STYLED_ITEM('',(#10486),#493);
#464=STYLED_ITEM('',(#10486),#494);
#465=STYLED_ITEM('',(#10486),#495);
#466=STYLED_ITEM('',(#10514),#496);
#467=STYLED_ITEM('',(#10493),#497);
#468=STYLED_ITEM('',(#10507),#378);
#469=STYLED_ITEM('',(#10507),#498);
#470=STYLED_ITEM('',(#10507),#499);
#471=STYLED_ITEM('',(#10486),#500);
#472=STYLED_ITEM('',(#10493),#501);
#473=STYLED_ITEM('',(#10514),#502);
#474=STYLED_ITEM('',(#10493),#503);
#475=STYLED_ITEM('',(#10507),#504);
#476=STYLED_ITEM('',(#10507),#379);
#477=MANIFOLD_SOLID_BREP('Body1',#5516);
#478=MANIFOLD_SOLID_BREP('Body1',#5517);
#479=MANIFOLD_SOLID_BREP('Body1',#5518);
#480=MANIFOLD_SOLID_BREP('Body1',#5519);
#481=MANIFOLD_SOLID_BREP('Body1',#5520);
#482=MANIFOLD_SOLID_BREP('Body1',#5521);
#483=MANIFOLD_SOLID_BREP('Body1',#5522);
#484=MANIFOLD_SOLID_BREP('Body1',#5523);
#485=MANIFOLD_SOLID_BREP('Body1',#5526);
#486=MANIFOLD_SOLID_BREP('Body1',#5527);
#487=MANIFOLD_SOLID_BREP('Body1',#5528);
#488=MANIFOLD_SOLID_BREP('Body1',#5531);
#489=MANIFOLD_SOLID_BREP('Body1',#5532);
#490=MANIFOLD_SOLID_BREP('Body1',#5533);
#491=MANIFOLD_SOLID_BREP('Body1',#5534);
#492=MANIFOLD_SOLID_BREP('Body1',#5535);
#493=MANIFOLD_SOLID_BREP('Body1',#5536);
#494=MANIFOLD_SOLID_BREP('Body1',#5537);
#495=MANIFOLD_SOLID_BREP('Body1',#5538);
#496=MANIFOLD_SOLID_BREP('Body1',#5539);
#497=MANIFOLD_SOLID_BREP('Body1',#5540);
#498=MANIFOLD_SOLID_BREP('Body1',#5543);
#499=MANIFOLD_SOLID_BREP('Body1',#5544);
#500=MANIFOLD_SOLID_BREP('Body1',#5545);
#501=MANIFOLD_SOLID_BREP('Body1',#5546);
#502=MANIFOLD_SOLID_BREP('Body1',#5547);
#503=MANIFOLD_SOLID_BREP('Body1',#5548);
#504=MANIFOLD_SOLID_BREP('Body1',#5549);
#505=SPHERICAL_SURFACE('',#5944,1.6);
#506=SPHERICAL_SURFACE('',#5987,1.6);
#507=SPHERICAL_SURFACE('',#6082,1.5);
#508=SPHERICAL_SURFACE('',#6317,0.837);
#509=SPHERICAL_SURFACE('',#6331,1.2);
#510=SPHERICAL_SURFACE('',#6523,1.5);
#511=FACE_BOUND('',#1178,.T.);
#512=FACE_BOUND('',#1179,.T.);
#513=FACE_BOUND('',#1183,.T.);
#514=FACE_BOUND('',#1185,.T.);
#515=FACE_BOUND('',#1187,.T.);
#516=FACE_BOUND('',#1189,.T.);
#517=FACE_BOUND('',#1190,.T.);
#518=FACE_BOUND('',#1191,.T.);
#519=FACE_BOUND('',#1192,.T.);
#520=FACE_BOUND('',#1195,.T.);
#521=FACE_BOUND('',#1196,.T.);
#522=FACE_BOUND('',#1197,.T.);
#523=FACE_BOUND('',#1198,.T.);
#524=FACE_BOUND('',#1199,.T.);
#525=FACE_BOUND('',#1213,.T.);
#526=FACE_BOUND('',#1214,.T.);
#527=FACE_BOUND('',#1218,.T.);
#528=FACE_BOUND('',#1220,.T.);
#529=FACE_BOUND('',#1222,.T.);
#530=FACE_BOUND('',#1224,.T.);
#531=FACE_BOUND('',#1225,.T.);
#532=FACE_BOUND('',#1226,.T.);
#533=FACE_BOUND('',#1227,.T.);
#534=FACE_BOUND('',#1228,.T.);
#535=FACE_BOUND('',#1231,.T.);
#536=FACE_BOUND('',#1232,.T.);
#537=FACE_BOUND('',#1233,.T.);
#538=FACE_BOUND('',#1234,.T.);
#539=FACE_BOUND('',#1246,.T.);
#540=FACE_BOUND('',#1247,.T.);
#541=FACE_BOUND('',#1248,.T.);
#542=FACE_BOUND('',#1249,.T.);
#543=FACE_BOUND('',#1257,.T.);
#544=FACE_BOUND('',#1258,.T.);
#545=FACE_BOUND('',#1259,.T.);
#546=FACE_BOUND('',#1260,.T.);
#547=FACE_BOUND('',#1262,.T.);
#548=FACE_BOUND('',#1265,.T.);
#549=FACE_BOUND('',#1269,.T.);
#550=FACE_BOUND('',#1273,.T.);
#551=FACE_BOUND('',#1277,.T.);
#552=FACE_BOUND('',#1279,.T.);
#553=FACE_BOUND('',#1294,.T.);
#554=FACE_BOUND('',#1295,.T.);
#555=FACE_BOUND('',#1296,.T.);
#556=FACE_BOUND('',#1297,.T.);
#557=FACE_BOUND('',#1298,.T.);
#558=FACE_BOUND('',#1299,.T.);
#559=FACE_BOUND('',#1300,.T.);
#560=FACE_BOUND('',#1302,.T.);
#561=FACE_BOUND('',#1303,.T.);
#562=FACE_BOUND('',#1304,.T.);
#563=FACE_BOUND('',#1305,.T.);
#564=FACE_BOUND('',#1306,.T.);
#565=FACE_BOUND('',#1308,.T.);
#566=FACE_BOUND('',#1312,.T.);
#567=FACE_BOUND('',#1314,.T.);
#568=FACE_BOUND('',#1324,.T.);
#569=FACE_BOUND('',#1332,.T.);
#570=FACE_BOUND('',#1338,.T.);
#571=FACE_BOUND('',#1341,.T.);
#572=FACE_BOUND('',#1352,.T.);
#573=FACE_BOUND('',#1354,.T.);
#574=FACE_BOUND('',#1358,.T.);
#575=FACE_BOUND('',#1360,.T.);
#576=FACE_BOUND('',#1366,.T.);
#577=FACE_BOUND('',#1385,.T.);
#578=FACE_BOUND('',#1387,.T.);
#579=FACE_BOUND('',#1404,.T.);
#580=FACE_BOUND('',#1407,.T.);
#581=FACE_BOUND('',#1409,.T.);
#582=FACE_BOUND('',#1413,.T.);
#583=FACE_BOUND('',#1415,.T.);
#584=FACE_BOUND('',#1419,.T.);
#585=FACE_BOUND('',#1421,.T.);
#586=FACE_BOUND('',#1425,.T.);
#587=FACE_BOUND('',#1427,.T.);
#588=FACE_BOUND('',#1430,.T.);
#589=FACE_BOUND('',#1433,.T.);
#590=FACE_BOUND('',#1437,.T.);
#591=FACE_BOUND('',#1441,.T.);
#592=FACE_BOUND('',#1444,.T.);
#593=FACE_BOUND('',#1446,.T.);
#594=FACE_BOUND('',#1449,.T.);
#595=FACE_BOUND('',#1452,.T.);
#596=FACE_BOUND('',#1454,.T.);
#597=FACE_BOUND('',#1463,.T.);
#598=FACE_BOUND('',#1468,.T.);
#599=FACE_BOUND('',#1475,.T.);
#600=FACE_BOUND('',#1476,.T.);
#601=FACE_BOUND('',#1477,.T.);
#602=FACE_BOUND('',#1478,.T.);
#603=FACE_BOUND('',#1479,.T.);
#604=FACE_BOUND('',#1484,.T.);
#605=FACE_BOUND('',#1485,.T.);
#606=FACE_BOUND('',#1486,.T.);
#607=FACE_BOUND('',#1487,.T.);
#608=FACE_BOUND('',#1488,.T.);
#609=FACE_BOUND('',#1490,.T.);
#610=FACE_BOUND('',#1496,.T.);
#611=FACE_BOUND('',#1497,.T.);
#612=FACE_BOUND('',#1498,.T.);
#613=FACE_BOUND('',#1499,.T.);
#614=FACE_BOUND('',#1500,.T.);
#615=FACE_BOUND('',#1505,.T.);
#616=FACE_BOUND('',#1507,.T.);
#617=FACE_BOUND('',#1508,.T.);
#618=FACE_BOUND('',#1509,.T.);
#619=FACE_BOUND('',#1510,.T.);
#620=FACE_BOUND('',#1511,.T.);
#621=FACE_BOUND('',#1517,.T.);
#622=FACE_BOUND('',#1533,.T.);
#623=FACE_BOUND('',#1535,.T.);
#624=FACE_BOUND('',#1546,.T.);
#625=FACE_BOUND('',#1548,.T.);
#626=FACE_BOUND('',#1556,.T.);
#627=FACE_BOUND('',#1557,.T.);
#628=FACE_BOUND('',#1569,.T.);
#629=FACE_BOUND('',#1581,.T.);
#630=FACE_BOUND('',#1591,.T.);
#631=FACE_BOUND('',#1593,.T.);
#632=FACE_BOUND('',#1597,.T.);
#633=FACE_BOUND('',#1599,.T.);
#634=FACE_BOUND('',#1620,.T.);
#635=PLANE('',#5912);
#636=PLANE('',#5916);
#637=PLANE('',#5932);
#638=PLANE('',#5934);
#639=PLANE('',#5941);
#640=PLANE('',#5943);
#641=PLANE('',#5946);
#642=PLANE('',#5947);
#643=PLANE('',#5948);
#644=PLANE('',#5949);
#645=PLANE('',#5950);
#646=PLANE('',#5955);
#647=PLANE('',#5959);
#648=PLANE('',#5975);
#649=PLANE('',#5977);
#650=PLANE('',#5984);
#651=PLANE('',#5985);
#652=PLANE('',#5989);
#653=PLANE('',#5990);
#654=PLANE('',#5991);
#655=PLANE('',#5992);
#656=PLANE('',#5993);
#657=PLANE('',#6007);
#658=PLANE('',#6008);
#659=PLANE('',#6009);
#660=PLANE('',#6010);
#661=PLANE('',#6011);
#662=PLANE('',#6013);
#663=PLANE('',#6014);
#664=PLANE('',#6017);
#665=PLANE('',#6018);
#666=PLANE('',#6019);
#667=PLANE('',#6020);
#668=PLANE('',#6022);
#669=PLANE('',#6027);
#670=PLANE('',#6033);
#671=PLANE('',#6042);
#672=PLANE('',#6049);
#673=PLANE('',#6050);
#674=PLANE('',#6055);
#675=PLANE('',#6059);
#676=PLANE('',#6075);
#677=PLANE('',#6076);
#678=PLANE('',#6077);
#679=PLANE('',#6078);
#680=PLANE('',#6079);
#681=PLANE('',#6080);
#682=PLANE('',#6090);
#683=PLANE('',#6091);
#684=PLANE('',#6093);
#685=PLANE('',#6094);
#686=PLANE('',#6095);
#687=PLANE('',#6096);
#688=PLANE('',#6097);
#689=PLANE('',#6098);
#690=PLANE('',#6099);
#691=PLANE('',#6100);
#692=PLANE('',#6101);
#693=PLANE('',#6106);
#694=PLANE('',#6107);
#695=PLANE('',#6115);
#696=PLANE('',#6126);
#697=PLANE('',#6130);
#698=PLANE('',#6136);
#699=PLANE('',#6137);
#700=PLANE('',#6138);
#701=PLANE('',#6142);
#702=PLANE('',#6143);
#703=PLANE('',#6144);
#704=PLANE('',#6145);
#705=PLANE('',#6146);
#706=PLANE('',#6154);
#707=PLANE('',#6155);
#708=PLANE('',#6157);
#709=PLANE('',#6165);
#710=PLANE('',#6173);
#711=PLANE('',#6174);
#712=PLANE('',#6175);
#713=PLANE('',#6176);
#714=PLANE('',#6177);
#715=PLANE('',#6178);
#716=PLANE('',#6179);
#717=PLANE('',#6180);
#718=PLANE('',#6181);
#719=PLANE('',#6186);
#720=PLANE('',#6187);
#721=PLANE('',#6230);
#722=PLANE('',#6231);
#723=PLANE('',#6233);
#724=PLANE('',#6242);
#725=PLANE('',#6251);
#726=PLANE('',#6256);
#727=PLANE('',#6267);
#728=PLANE('',#6272);
#729=PLANE('',#6278);
#730=PLANE('',#6282);
#731=PLANE('',#6283);
#732=PLANE('',#6291);
#733=PLANE('',#6292);
#734=PLANE('',#6300);
#735=PLANE('',#6301);
#736=PLANE('',#6309);
#737=PLANE('',#6310);
#738=PLANE('',#6323);
#739=PLANE('',#6330);
#740=PLANE('',#6339);
#741=PLANE('',#6343);
#742=PLANE('',#6344);
#743=PLANE('',#6349);
#744=PLANE('',#6352);
#745=PLANE('',#6354);
#746=PLANE('',#6356);
#747=PLANE('',#6357);
#748=PLANE('',#6358);
#749=PLANE('',#6359);
#750=PLANE('',#6360);
#751=PLANE('',#6361);
#752=PLANE('',#6364);
#753=PLANE('',#6372);
#754=PLANE('',#6388);
#755=PLANE('',#6398);
#756=PLANE('',#6399);
#757=PLANE('',#6413);
#758=PLANE('',#6423);
#759=PLANE('',#6424);
#760=PLANE('',#6426);
#761=PLANE('',#6434);
#762=PLANE('',#6442);
#763=PLANE('',#6443);
#764=PLANE('',#6444);
#765=PLANE('',#6445);
#766=PLANE('',#6446);
#767=PLANE('',#6447);
#768=PLANE('',#6448);
#769=PLANE('',#6449);
#770=PLANE('',#6450);
#771=PLANE('',#6458);
#772=PLANE('',#6459);
#773=PLANE('',#6465);
#774=PLANE('',#6466);
#775=PLANE('',#6467);
#776=PLANE('',#6471);
#777=PLANE('',#6472);
#778=PLANE('',#6473);
#779=PLANE('',#6474);
#780=PLANE('',#6475);
#781=PLANE('',#6510);
#782=PLANE('',#6512);
#783=PLANE('',#6515);
#784=PLANE('',#6517);
#785=PLANE('',#6519);
#786=PLANE('',#6529);
#787=PLANE('',#6530);
#788=PLANE('',#6532);
#789=PLANE('',#6534);
#790=PLANE('',#6536);
#791=PLANE('',#6538);
#792=PLANE('',#6539);
#793=PLANE('',#6540);
#794=PLANE('',#6541);
#795=PLANE('',#6542);
#796=PLANE('',#6543);
#797=PLANE('',#6545);
#798=PLANE('',#6548);
#799=PLANE('',#6550);
#800=PLANE('',#6552);
#801=PLANE('',#6553);
#802=PLANE('',#6554);
#803=PLANE('',#6555);
#804=PLANE('',#6556);
#805=PLANE('',#6559);
#806=PLANE('',#6561);
#807=PLANE('',#6562);
#808=PLANE('',#6563);
#809=PLANE('',#6564);
#810=PLANE('',#6565);
#811=PLANE('',#6566);
#812=PLANE('',#6567);
#813=PLANE('',#6568);
#814=PLANE('',#6569);
#815=PLANE('',#6570);
#816=PLANE('',#6578);
#817=PLANE('',#6579);
#818=PLANE('',#6581);
#819=PLANE('',#6582);
#820=PLANE('',#6583);
#821=PLANE('',#6584);
#822=PLANE('',#6585);
#823=PLANE('',#6586);
#824=PLANE('',#6588);
#825=PLANE('',#6589);
#826=PLANE('',#6590);
#827=PLANE('',#6591);
#828=PLANE('',#6592);
#829=PLANE('',#6593);
#830=PLANE('',#6594);
#831=PLANE('',#6595);
#832=PLANE('',#6596);
#833=PLANE('',#6598);
#834=PLANE('',#6606);
#835=FACE_OUTER_BOUND('',#1167,.T.);
#836=FACE_OUTER_BOUND('',#1168,.T.);
#837=FACE_OUTER_BOUND('',#1169,.T.);
#838=FACE_OUTER_BOUND('',#1170,.T.);
#839=FACE_OUTER_BOUND('',#1171,.T.);
#840=FACE_OUTER_BOUND('',#1172,.T.);
#841=FACE_OUTER_BOUND('',#1173,.T.);
#842=FACE_OUTER_BOUND('',#1174,.T.);
#843=FACE_OUTER_BOUND('',#1175,.T.);
#844=FACE_OUTER_BOUND('',#1176,.T.);
#845=FACE_OUTER_BOUND('',#1177,.T.);
#846=FACE_OUTER_BOUND('',#1180,.T.);
#847=FACE_OUTER_BOUND('',#1181,.T.);
#848=FACE_OUTER_BOUND('',#1182,.T.);
#849=FACE_OUTER_BOUND('',#1184,.T.);
#850=FACE_OUTER_BOUND('',#1186,.T.);
#851=FACE_OUTER_BOUND('',#1188,.T.);
#852=FACE_OUTER_BOUND('',#1193,.T.);
#853=FACE_OUTER_BOUND('',#1194,.T.);
#854=FACE_OUTER_BOUND('',#1200,.T.);
#855=FACE_OUTER_BOUND('',#1201,.T.);
#856=FACE_OUTER_BOUND('',#1202,.T.);
#857=FACE_OUTER_BOUND('',#1203,.T.);
#858=FACE_OUTER_BOUND('',#1204,.T.);
#859=FACE_OUTER_BOUND('',#1205,.T.);
#860=FACE_OUTER_BOUND('',#1206,.T.);
#861=FACE_OUTER_BOUND('',#1207,.T.);
#862=FACE_OUTER_BOUND('',#1208,.T.);
#863=FACE_OUTER_BOUND('',#1209,.T.);
#864=FACE_OUTER_BOUND('',#1210,.T.);
#865=FACE_OUTER_BOUND('',#1211,.T.);
#866=FACE_OUTER_BOUND('',#1212,.T.);
#867=FACE_OUTER_BOUND('',#1215,.T.);
#868=FACE_OUTER_BOUND('',#1216,.T.);
#869=FACE_OUTER_BOUND('',#1217,.T.);
#870=FACE_OUTER_BOUND('',#1219,.T.);
#871=FACE_OUTER_BOUND('',#1221,.T.);
#872=FACE_OUTER_BOUND('',#1223,.T.);
#873=FACE_OUTER_BOUND('',#1229,.T.);
#874=FACE_OUTER_BOUND('',#1230,.T.);
#875=FACE_OUTER_BOUND('',#1235,.T.);
#876=FACE_OUTER_BOUND('',#1236,.T.);
#877=FACE_OUTER_BOUND('',#1237,.T.);
#878=FACE_OUTER_BOUND('',#1238,.T.);
#879=FACE_OUTER_BOUND('',#1239,.T.);
#880=FACE_OUTER_BOUND('',#1240,.T.);
#881=FACE_OUTER_BOUND('',#1241,.T.);
#882=FACE_OUTER_BOUND('',#1242,.T.);
#883=FACE_OUTER_BOUND('',#1243,.T.);
#884=FACE_OUTER_BOUND('',#1244,.T.);
#885=FACE_OUTER_BOUND('',#1245,.T.);
#886=FACE_OUTER_BOUND('',#1250,.T.);
#887=FACE_OUTER_BOUND('',#1251,.T.);
#888=FACE_OUTER_BOUND('',#1252,.T.);
#889=FACE_OUTER_BOUND('',#1253,.T.);
#890=FACE_OUTER_BOUND('',#1254,.T.);
#891=FACE_OUTER_BOUND('',#1255,.T.);
#892=FACE_OUTER_BOUND('',#1256,.T.);
#893=FACE_OUTER_BOUND('',#1261,.T.);
#894=FACE_OUTER_BOUND('',#1263,.T.);
#895=FACE_OUTER_BOUND('',#1264,.T.);
#896=FACE_OUTER_BOUND('',#1266,.T.);
#897=FACE_OUTER_BOUND('',#1267,.T.);
#898=FACE_OUTER_BOUND('',#1268,.T.);
#899=FACE_OUTER_BOUND('',#1270,.T.);
#900=FACE_OUTER_BOUND('',#1271,.T.);
#901=FACE_OUTER_BOUND('',#1272,.T.);
#902=FACE_OUTER_BOUND('',#1274,.T.);
#903=FACE_OUTER_BOUND('',#1275,.T.);
#904=FACE_OUTER_BOUND('',#1276,.T.);
#905=FACE_OUTER_BOUND('',#1278,.T.);
#906=FACE_OUTER_BOUND('',#1280,.T.);
#907=FACE_OUTER_BOUND('',#1281,.T.);
#908=FACE_OUTER_BOUND('',#1282,.T.);
#909=FACE_OUTER_BOUND('',#1283,.T.);
#910=FACE_OUTER_BOUND('',#1284,.T.);
#911=FACE_OUTER_BOUND('',#1285,.T.);
#912=FACE_OUTER_BOUND('',#1286,.T.);
#913=FACE_OUTER_BOUND('',#1287,.T.);
#914=FACE_OUTER_BOUND('',#1288,.T.);
#915=FACE_OUTER_BOUND('',#1289,.T.);
#916=FACE_OUTER_BOUND('',#1290,.T.);
#917=FACE_OUTER_BOUND('',#1291,.T.);
#918=FACE_OUTER_BOUND('',#1292,.T.);
#919=FACE_OUTER_BOUND('',#1293,.T.);
#920=FACE_OUTER_BOUND('',#1301,.T.);
#921=FACE_OUTER_BOUND('',#1307,.T.);
#922=FACE_OUTER_BOUND('',#1309,.T.);
#923=FACE_OUTER_BOUND('',#1310,.T.);
#924=FACE_OUTER_BOUND('',#1311,.T.);
#925=FACE_OUTER_BOUND('',#1313,.T.);
#926=FACE_OUTER_BOUND('',#1315,.T.);
#927=FACE_OUTER_BOUND('',#1316,.T.);
#928=FACE_OUTER_BOUND('',#1317,.T.);
#929=FACE_OUTER_BOUND('',#1318,.T.);
#930=FACE_OUTER_BOUND('',#1319,.T.);
#931=FACE_OUTER_BOUND('',#1320,.T.);
#932=FACE_OUTER_BOUND('',#1321,.T.);
#933=FACE_OUTER_BOUND('',#1322,.T.);
#934=FACE_OUTER_BOUND('',#1323,.T.);
#935=FACE_OUTER_BOUND('',#1325,.T.);
#936=FACE_OUTER_BOUND('',#1326,.T.);
#937=FACE_OUTER_BOUND('',#1327,.T.);
#938=FACE_OUTER_BOUND('',#1328,.T.);
#939=FACE_OUTER_BOUND('',#1329,.T.);
#940=FACE_OUTER_BOUND('',#1330,.T.);
#941=FACE_OUTER_BOUND('',#1331,.T.);
#942=FACE_OUTER_BOUND('',#1333,.T.);
#943=FACE_OUTER_BOUND('',#1334,.T.);
#944=FACE_OUTER_BOUND('',#1335,.T.);
#945=FACE_OUTER_BOUND('',#1336,.T.);
#946=FACE_OUTER_BOUND('',#1337,.T.);
#947=FACE_OUTER_BOUND('',#1339,.T.);
#948=FACE_OUTER_BOUND('',#1340,.T.);
#949=FACE_OUTER_BOUND('',#1342,.T.);
#950=FACE_OUTER_BOUND('',#1343,.T.);
#951=FACE_OUTER_BOUND('',#1344,.T.);
#952=FACE_OUTER_BOUND('',#1345,.T.);
#953=FACE_OUTER_BOUND('',#1346,.T.);
#954=FACE_OUTER_BOUND('',#1347,.T.);
#955=FACE_OUTER_BOUND('',#1348,.T.);
#956=FACE_OUTER_BOUND('',#1349,.T.);
#957=FACE_OUTER_BOUND('',#1350,.T.);
#958=FACE_OUTER_BOUND('',#1351,.T.);
#959=FACE_OUTER_BOUND('',#1353,.T.);
#960=FACE_OUTER_BOUND('',#1355,.T.);
#961=FACE_OUTER_BOUND('',#1356,.T.);
#962=FACE_OUTER_BOUND('',#1357,.T.);
#963=FACE_OUTER_BOUND('',#1359,.T.);
#964=FACE_OUTER_BOUND('',#1361,.T.);
#965=FACE_OUTER_BOUND('',#1362,.T.);
#966=FACE_OUTER_BOUND('',#1363,.T.);
#967=FACE_OUTER_BOUND('',#1364,.T.);
#968=FACE_OUTER_BOUND('',#1365,.T.);
#969=FACE_OUTER_BOUND('',#1367,.T.);
#970=FACE_OUTER_BOUND('',#1368,.T.);
#971=FACE_OUTER_BOUND('',#1369,.T.);
#972=FACE_OUTER_BOUND('',#1370,.T.);
#973=FACE_OUTER_BOUND('',#1371,.T.);
#974=FACE_OUTER_BOUND('',#1372,.T.);
#975=FACE_OUTER_BOUND('',#1373,.T.);
#976=FACE_OUTER_BOUND('',#1374,.T.);
#977=FACE_OUTER_BOUND('',#1375,.T.);
#978=FACE_OUTER_BOUND('',#1376,.T.);
#979=FACE_OUTER_BOUND('',#1377,.T.);
#980=FACE_OUTER_BOUND('',#1378,.T.);
#981=FACE_OUTER_BOUND('',#1379,.T.);
#982=FACE_OUTER_BOUND('',#1380,.T.);
#983=FACE_OUTER_BOUND('',#1381,.T.);
#984=FACE_OUTER_BOUND('',#1382,.T.);
#985=FACE_OUTER_BOUND('',#1383,.T.);
#986=FACE_OUTER_BOUND('',#1384,.T.);
#987=FACE_OUTER_BOUND('',#1386,.T.);
#988=FACE_OUTER_BOUND('',#1388,.T.);
#989=FACE_OUTER_BOUND('',#1389,.T.);
#990=FACE_OUTER_BOUND('',#1390,.T.);
#991=FACE_OUTER_BOUND('',#1391,.T.);
#992=FACE_OUTER_BOUND('',#1392,.T.);
#993=FACE_OUTER_BOUND('',#1393,.T.);
#994=FACE_OUTER_BOUND('',#1394,.T.);
#995=FACE_OUTER_BOUND('',#1395,.T.);
#996=FACE_OUTER_BOUND('',#1396,.T.);
#997=FACE_OUTER_BOUND('',#1397,.T.);
#998=FACE_OUTER_BOUND('',#1398,.T.);
#999=FACE_OUTER_BOUND('',#1399,.T.);
#1000=FACE_OUTER_BOUND('',#1400,.T.);
#1001=FACE_OUTER_BOUND('',#1401,.T.);
#1002=FACE_OUTER_BOUND('',#1402,.T.);
#1003=FACE_OUTER_BOUND('',#1403,.T.);
#1004=FACE_OUTER_BOUND('',#1405,.T.);
#1005=FACE_OUTER_BOUND('',#1406,.T.);
#1006=FACE_OUTER_BOUND('',#1408,.T.);
#1007=FACE_OUTER_BOUND('',#1410,.T.);
#1008=FACE_OUTER_BOUND('',#1411,.T.);
#1009=FACE_OUTER_BOUND('',#1412,.T.);
#1010=FACE_OUTER_BOUND('',#1414,.T.);
#1011=FACE_OUTER_BOUND('',#1416,.T.);
#1012=FACE_OUTER_BOUND('',#1417,.T.);
#1013=FACE_OUTER_BOUND('',#1418,.T.);
#1014=FACE_OUTER_BOUND('',#1420,.T.);
#1015=FACE_OUTER_BOUND('',#1422,.T.);
#1016=FACE_OUTER_BOUND('',#1423,.T.);
#1017=FACE_OUTER_BOUND('',#1424,.T.);
#1018=FACE_OUTER_BOUND('',#1426,.T.);
#1019=FACE_OUTER_BOUND('',#1428,.T.);
#1020=FACE_OUTER_BOUND('',#1429,.T.);
#1021=FACE_OUTER_BOUND('',#1431,.T.);
#1022=FACE_OUTER_BOUND('',#1432,.T.);
#1023=FACE_OUTER_BOUND('',#1434,.T.);
#1024=FACE_OUTER_BOUND('',#1435,.T.);
#1025=FACE_OUTER_BOUND('',#1436,.T.);
#1026=FACE_OUTER_BOUND('',#1438,.T.);
#1027=FACE_OUTER_BOUND('',#1439,.T.);
#1028=FACE_OUTER_BOUND('',#1440,.T.);
#1029=FACE_OUTER_BOUND('',#1442,.T.);
#1030=FACE_OUTER_BOUND('',#1443,.T.);
#1031=FACE_OUTER_BOUND('',#1445,.T.);
#1032=FACE_OUTER_BOUND('',#1447,.T.);
#1033=FACE_OUTER_BOUND('',#1448,.T.);
#1034=FACE_OUTER_BOUND('',#1450,.T.);
#1035=FACE_OUTER_BOUND('',#1451,.T.);
#1036=FACE_OUTER_BOUND('',#1453,.T.);
#1037=FACE_OUTER_BOUND('',#1455,.T.);
#1038=FACE_OUTER_BOUND('',#1456,.T.);
#1039=FACE_OUTER_BOUND('',#1457,.T.);
#1040=FACE_OUTER_BOUND('',#1458,.T.);
#1041=FACE_OUTER_BOUND('',#1459,.T.);
#1042=FACE_OUTER_BOUND('',#1460,.T.);
#1043=FACE_OUTER_BOUND('',#1461,.T.);
#1044=FACE_OUTER_BOUND('',#1462,.T.);
#1045=FACE_OUTER_BOUND('',#1464,.T.);
#1046=FACE_OUTER_BOUND('',#1465,.T.);
#1047=FACE_OUTER_BOUND('',#1466,.T.);
#1048=FACE_OUTER_BOUND('',#1467,.T.);
#1049=FACE_OUTER_BOUND('',#1469,.T.);
#1050=FACE_OUTER_BOUND('',#1470,.T.);
#1051=FACE_OUTER_BOUND('',#1471,.T.);
#1052=FACE_OUTER_BOUND('',#1472,.T.);
#1053=FACE_OUTER_BOUND('',#1473,.T.);
#1054=FACE_OUTER_BOUND('',#1474,.T.);
#1055=FACE_OUTER_BOUND('',#1480,.T.);
#1056=FACE_OUTER_BOUND('',#1481,.T.);
#1057=FACE_OUTER_BOUND('',#1482,.T.);
#1058=FACE_OUTER_BOUND('',#1483,.T.);
#1059=FACE_OUTER_BOUND('',#1489,.T.);
#1060=FACE_OUTER_BOUND('',#1491,.T.);
#1061=FACE_OUTER_BOUND('',#1492,.T.);
#1062=FACE_OUTER_BOUND('',#1493,.T.);
#1063=FACE_OUTER_BOUND('',#1494,.T.);
#1064=FACE_OUTER_BOUND('',#1495,.T.);
#1065=FACE_OUTER_BOUND('',#1501,.T.);
#1066=FACE_OUTER_BOUND('',#1502,.T.);
#1067=FACE_OUTER_BOUND('',#1503,.T.);
#1068=FACE_OUTER_BOUND('',#1504,.T.);
#1069=FACE_OUTER_BOUND('',#1506,.T.);
#1070=FACE_OUTER_BOUND('',#1512,.T.);
#1071=FACE_OUTER_BOUND('',#1513,.T.);
#1072=FACE_OUTER_BOUND('',#1514,.T.);
#1073=FACE_OUTER_BOUND('',#1515,.T.);
#1074=FACE_OUTER_BOUND('',#1516,.T.);
#1075=FACE_OUTER_BOUND('',#1518,.T.);
#1076=FACE_OUTER_BOUND('',#1519,.T.);
#1077=FACE_OUTER_BOUND('',#1520,.T.);
#1078=FACE_OUTER_BOUND('',#1521,.T.);
#1079=FACE_OUTER_BOUND('',#1522,.T.);
#1080=FACE_OUTER_BOUND('',#1523,.T.);
#1081=FACE_OUTER_BOUND('',#1524,.T.);
#1082=FACE_OUTER_BOUND('',#1525,.T.);
#1083=FACE_OUTER_BOUND('',#1526,.T.);
#1084=FACE_OUTER_BOUND('',#1527,.T.);
#1085=FACE_OUTER_BOUND('',#1528,.T.);
#1086=FACE_OUTER_BOUND('',#1529,.T.);
#1087=FACE_OUTER_BOUND('',#1530,.T.);
#1088=FACE_OUTER_BOUND('',#1531,.T.);
#1089=FACE_OUTER_BOUND('',#1532,.T.);
#1090=FACE_OUTER_BOUND('',#1534,.T.);
#1091=FACE_OUTER_BOUND('',#1536,.T.);
#1092=FACE_OUTER_BOUND('',#1537,.T.);
#1093=FACE_OUTER_BOUND('',#1538,.T.);
#1094=FACE_OUTER_BOUND('',#1539,.T.);
#1095=FACE_OUTER_BOUND('',#1540,.T.);
#1096=FACE_OUTER_BOUND('',#1541,.T.);
#1097=FACE_OUTER_BOUND('',#1542,.T.);
#1098=FACE_OUTER_BOUND('',#1543,.T.);
#1099=FACE_OUTER_BOUND('',#1544,.T.);
#1100=FACE_OUTER_BOUND('',#1545,.T.);
#1101=FACE_OUTER_BOUND('',#1547,.T.);
#1102=FACE_OUTER_BOUND('',#1549,.T.);
#1103=FACE_OUTER_BOUND('',#1550,.T.);
#1104=FACE_OUTER_BOUND('',#1551,.T.);
#1105=FACE_OUTER_BOUND('',#1552,.T.);
#1106=FACE_OUTER_BOUND('',#1553,.T.);
#1107=FACE_OUTER_BOUND('',#1554,.T.);
#1108=FACE_OUTER_BOUND('',#1555,.T.);
#1109=FACE_OUTER_BOUND('',#1558,.T.);
#1110=FACE_OUTER_BOUND('',#1559,.T.);
#1111=FACE_OUTER_BOUND('',#1560,.T.);
#1112=FACE_OUTER_BOUND('',#1561,.T.);
#1113=FACE_OUTER_BOUND('',#1562,.T.);
#1114=FACE_OUTER_BOUND('',#1563,.T.);
#1115=FACE_OUTER_BOUND('',#1564,.T.);
#1116=FACE_OUTER_BOUND('',#1565,.T.);
#1117=FACE_OUTER_BOUND('',#1566,.T.);
#1118=FACE_OUTER_BOUND('',#1567,.T.);
#1119=FACE_OUTER_BOUND('',#1568,.T.);
#1120=FACE_OUTER_BOUND('',#1570,.T.);
#1121=FACE_OUTER_BOUND('',#1571,.T.);
#1122=FACE_OUTER_BOUND('',#1572,.T.);
#1123=FACE_OUTER_BOUND('',#1573,.T.);
#1124=FACE_OUTER_BOUND('',#1574,.T.);
#1125=FACE_OUTER_BOUND('',#1575,.T.);
#1126=FACE_OUTER_BOUND('',#1576,.T.);
#1127=FACE_OUTER_BOUND('',#1577,.T.);
#1128=FACE_OUTER_BOUND('',#1578,.T.);
#1129=FACE_OUTER_BOUND('',#1579,.T.);
#1130=FACE_OUTER_BOUND('',#1580,.T.);
#1131=FACE_OUTER_BOUND('',#1582,.T.);
#1132=FACE_OUTER_BOUND('',#1583,.T.);
#1133=FACE_OUTER_BOUND('',#1584,.T.);
#1134=FACE_OUTER_BOUND('',#1585,.T.);
#1135=FACE_OUTER_BOUND('',#1586,.T.);
#1136=FACE_OUTER_BOUND('',#1587,.T.);
#1137=FACE_OUTER_BOUND('',#1588,.T.);
#1138=FACE_OUTER_BOUND('',#1589,.T.);
#1139=FACE_OUTER_BOUND('',#1590,.T.);
#1140=FACE_OUTER_BOUND('',#1592,.T.);
#1141=FACE_OUTER_BOUND('',#1594,.T.);
#1142=FACE_OUTER_BOUND('',#1595,.T.);
#1143=FACE_OUTER_BOUND('',#1596,.T.);
#1144=FACE_OUTER_BOUND('',#1598,.T.);
#1145=FACE_OUTER_BOUND('',#1600,.T.);
#1146=FACE_OUTER_BOUND('',#1601,.T.);
#1147=FACE_OUTER_BOUND('',#1602,.T.);
#1148=FACE_OUTER_BOUND('',#1603,.T.);
#1149=FACE_OUTER_BOUND('',#1604,.T.);
#1150=FACE_OUTER_BOUND('',#1605,.T.);
#1151=FACE_OUTER_BOUND('',#1606,.T.);
#1152=FACE_OUTER_BOUND('',#1607,.T.);
#1153=FACE_OUTER_BOUND('',#1608,.T.);
#1154=FACE_OUTER_BOUND('',#1609,.T.);
#1155=FACE_OUTER_BOUND('',#1610,.T.);
#1156=FACE_OUTER_BOUND('',#1611,.T.);
#1157=FACE_OUTER_BOUND('',#1612,.T.);
#1158=FACE_OUTER_BOUND('',#1613,.T.);
#1159=FACE_OUTER_BOUND('',#1614,.T.);
#1160=FACE_OUTER_BOUND('',#1615,.T.);
#1161=FACE_OUTER_BOUND('',#1616,.T.);
#1162=FACE_OUTER_BOUND('',#1617,.T.);
#1163=FACE_OUTER_BOUND('',#1618,.T.);
#1164=FACE_OUTER_BOUND('',#1619,.T.);
#1165=FACE_OUTER_BOUND('',#1621,.T.);
#1166=FACE_OUTER_BOUND('',#1622,.T.);
#1167=EDGE_LOOP('',(#3738,#3739,#3740,#3741));
#1168=EDGE_LOOP('',(#3742));
#1169=EDGE_LOOP('',(#3743,#3744,#3745,#3746));
#1170=EDGE_LOOP('',(#3747));
#1171=EDGE_LOOP('',(#3748,#3749,#3750,#3751));
#1172=EDGE_LOOP('',(#3752,#3753,#3754,#3755));
#1173=EDGE_LOOP('',(#3756,#3757,#3758,#3759));
#1174=EDGE_LOOP('',(#3760,#3761,#3762,#3763));
#1175=EDGE_LOOP('',(#3764,#3765,#3766,#3767));
#1176=EDGE_LOOP('',(#3768,#3769,#3770,#3771));
#1177=EDGE_LOOP('',(#3772,#3773,#3774,#3775,#3776,#3777));
#1178=EDGE_LOOP('',(#3778));
#1179=EDGE_LOOP('',(#3779));
#1180=EDGE_LOOP('',(#3780,#3781,#3782,#3783));
#1181=EDGE_LOOP('',(#3784,#3785,#3786,#3787));
#1182=EDGE_LOOP('',(#3788));
#1183=EDGE_LOOP('',(#3789));
#1184=EDGE_LOOP('',(#3790));
#1185=EDGE_LOOP('',(#3791));
#1186=EDGE_LOOP('',(#3792,#3793));
#1187=EDGE_LOOP('',(#3794));
#1188=EDGE_LOOP('',(#3795,#3796,#3797,#3798,#3799,#3800,#3801,#3802,#3803,
#3804));
#1189=EDGE_LOOP('',(#3805));
#1190=EDGE_LOOP('',(#3806));
#1191=EDGE_LOOP('',(#3807));
#1192=EDGE_LOOP('',(#3808));
#1193=EDGE_LOOP('',(#3809,#3810,#3811,#3812));
#1194=EDGE_LOOP('',(#3813,#3814,#3815,#3816));
#1195=EDGE_LOOP('',(#3817));
#1196=EDGE_LOOP('',(#3818));
#1197=EDGE_LOOP('',(#3819));
#1198=EDGE_LOOP('',(#3820));
#1199=EDGE_LOOP('',(#3821));
#1200=EDGE_LOOP('',(#3822,#3823,#3824,#3825));
#1201=EDGE_LOOP('',(#3826,#3827,#3828,#3829));
#1202=EDGE_LOOP('',(#3830,#3831,#3832,#3833));
#1203=EDGE_LOOP('',(#3834));
#1204=EDGE_LOOP('',(#3835,#3836,#3837,#3838));
#1205=EDGE_LOOP('',(#3839));
#1206=EDGE_LOOP('',(#3840,#3841,#3842,#3843));
#1207=EDGE_LOOP('',(#3844,#3845,#3846,#3847));
#1208=EDGE_LOOP('',(#3848,#3849,#3850,#3851));
#1209=EDGE_LOOP('',(#3852,#3853,#3854,#3855));
#1210=EDGE_LOOP('',(#3856,#3857,#3858,#3859));
#1211=EDGE_LOOP('',(#3860,#3861,#3862,#3863));
#1212=EDGE_LOOP('',(#3864,#3865,#3866,#3867,#3868,#3869));
#1213=EDGE_LOOP('',(#3870));
#1214=EDGE_LOOP('',(#3871));
#1215=EDGE_LOOP('',(#3872,#3873,#3874,#3875));
#1216=EDGE_LOOP('',(#3876,#3877,#3878,#3879));
#1217=EDGE_LOOP('',(#3880));
#1218=EDGE_LOOP('',(#3881));
#1219=EDGE_LOOP('',(#3882));
#1220=EDGE_LOOP('',(#3883));
#1221=EDGE_LOOP('',(#3884,#3885));
#1222=EDGE_LOOP('',(#3886));
#1223=EDGE_LOOP('',(#3887,#3888,#3889,#3890));
#1224=EDGE_LOOP('',(#3891));
#1225=EDGE_LOOP('',(#3892));
#1226=EDGE_LOOP('',(#3893));
#1227=EDGE_LOOP('',(#3894));
#1228=EDGE_LOOP('',(#3895));
#1229=EDGE_LOOP('',(#3896,#3897,#3898,#3899));
#1230=EDGE_LOOP('',(#3900,#3901,#3902,#3903,#3904,#3905,#3906,#3907,#3908,
#3909));
#1231=EDGE_LOOP('',(#3910));
#1232=EDGE_LOOP('',(#3911));
#1233=EDGE_LOOP('',(#3912));
#1234=EDGE_LOOP('',(#3913));
#1235=EDGE_LOOP('',(#3914,#3915,#3916,#3917));
#1236=EDGE_LOOP('',(#3918,#3919,#3920,#3921));
#1237=EDGE_LOOP('',(#3922,#3923,#3924,#3925));
#1238=EDGE_LOOP('',(#3926,#3927,#3928,#3929));
#1239=EDGE_LOOP('',(#3930,#3931,#3932,#3933));
#1240=EDGE_LOOP('',(#3934,#3935,#3936,#3937));
#1241=EDGE_LOOP('',(#3938,#3939,#3940,#3941));
#1242=EDGE_LOOP('',(#3942,#3943,#3944,#3945));
#1243=EDGE_LOOP('',(#3946,#3947,#3948,#3949));
#1244=EDGE_LOOP('',(#3950,#3951,#3952,#3953));
#1245=EDGE_LOOP('',(#3954,#3955,#3956,#3957,#3958,#3959,#3960,#3961,#3962,
#3963));
#1246=EDGE_LOOP('',(#3964));
#1247=EDGE_LOOP('',(#3965));
#1248=EDGE_LOOP('',(#3966));
#1249=EDGE_LOOP('',(#3967));
#1250=EDGE_LOOP('',(#3968,#3969,#3970,#3971));
#1251=EDGE_LOOP('',(#3972,#3973,#3974,#3975));
#1252=EDGE_LOOP('',(#3976,#3977,#3978,#3979));
#1253=EDGE_LOOP('',(#3980,#3981,#3982,#3983));
#1254=EDGE_LOOP('',(#3984,#3985,#3986,#3987));
#1255=EDGE_LOOP('',(#3988,#3989,#3990,#3991));
#1256=EDGE_LOOP('',(#3992,#3993,#3994,#3995,#3996,#3997,#3998,#3999,#4000,
#4001));
#1257=EDGE_LOOP('',(#4002));
#1258=EDGE_LOOP('',(#4003));
#1259=EDGE_LOOP('',(#4004));
#1260=EDGE_LOOP('',(#4005));
#1261=EDGE_LOOP('',(#4006));
#1262=EDGE_LOOP('',(#4007));
#1263=EDGE_LOOP('',(#4008,#4009,#4010,#4011));
#1264=EDGE_LOOP('',(#4012));
#1265=EDGE_LOOP('',(#4013));
#1266=EDGE_LOOP('',(#4014,#4015,#4016,#4017));
#1267=EDGE_LOOP('',(#4018,#4019,#4020,#4021));
#1268=EDGE_LOOP('',(#4022));
#1269=EDGE_LOOP('',(#4023));
#1270=EDGE_LOOP('',(#4024,#4025,#4026,#4027));
#1271=EDGE_LOOP('',(#4028,#4029,#4030,#4031));
#1272=EDGE_LOOP('',(#4032));
#1273=EDGE_LOOP('',(#4033));
#1274=EDGE_LOOP('',(#4034,#4035,#4036,#4037));
#1275=EDGE_LOOP('',(#4038,#4039,#4040,#4041));
#1276=EDGE_LOOP('',(#4042));
#1277=EDGE_LOOP('',(#4043));
#1278=EDGE_LOOP('',(#4044));
#1279=EDGE_LOOP('',(#4045));
#1280=EDGE_LOOP('',(#4046,#4047,#4048,#4049));
#1281=EDGE_LOOP('',(#4050));
#1282=EDGE_LOOP('',(#4051,#4052,#4053,#4054));
#1283=EDGE_LOOP('',(#4055));
#1284=EDGE_LOOP('',(#4056,#4057,#4058,#4059));
#1285=EDGE_LOOP('',(#4060,#4061,#4062,#4063));
#1286=EDGE_LOOP('',(#4064,#4065,#4066,#4067));
#1287=EDGE_LOOP('',(#4068,#4069,#4070,#4071));
#1288=EDGE_LOOP('',(#4072,#4073,#4074,#4075));
#1289=EDGE_LOOP('',(#4076,#4077,#4078,#4079));
#1290=EDGE_LOOP('',(#4080,#4081,#4082,#4083));
#1291=EDGE_LOOP('',(#4084,#4085,#4086,#4087));
#1292=EDGE_LOOP('',(#4088,#4089,#4090,#4091));
#1293=EDGE_LOOP('',(#4092,#4093,#4094,#4095));
#1294=EDGE_LOOP('',(#4096));
#1295=EDGE_LOOP('',(#4097));
#1296=EDGE_LOOP('',(#4098));
#1297=EDGE_LOOP('',(#4099));
#1298=EDGE_LOOP('',(#4100));
#1299=EDGE_LOOP('',(#4101));
#1300=EDGE_LOOP('',(#4102));
#1301=EDGE_LOOP('',(#4103,#4104,#4105,#4106));
#1302=EDGE_LOOP('',(#4107));
#1303=EDGE_LOOP('',(#4108));
#1304=EDGE_LOOP('',(#4109));
#1305=EDGE_LOOP('',(#4110));
#1306=EDGE_LOOP('',(#4111));
#1307=EDGE_LOOP('',(#4112));
#1308=EDGE_LOOP('',(#4113));
#1309=EDGE_LOOP('',(#4114,#4115,#4116,#4117));
#1310=EDGE_LOOP('',(#4118,#4119,#4120,#4121));
#1311=EDGE_LOOP('',(#4122));
#1312=EDGE_LOOP('',(#4123));
#1313=EDGE_LOOP('',(#4124));
#1314=EDGE_LOOP('',(#4125));
#1315=EDGE_LOOP('',(#4126,#4127,#4128,#4129));
#1316=EDGE_LOOP('',(#4130,#4131,#4132,#4133));
#1317=EDGE_LOOP('',(#4134,#4135,#4136,#4137));
#1318=EDGE_LOOP('',(#4138,#4139,#4140,#4141));
#1319=EDGE_LOOP('',(#4142,#4143,#4144,#4145));
#1320=EDGE_LOOP('',(#4146,#4147,#4148,#4149));
#1321=EDGE_LOOP('',(#4150,#4151,#4152,#4153,#4154,#4155));
#1322=EDGE_LOOP('',(#4156,#4157,#4158,#4159,#4160,#4161));
#1323=EDGE_LOOP('',(#4162));
#1324=EDGE_LOOP('',(#4163));
#1325=EDGE_LOOP('',(#4164,#4165,#4166,#4167));
#1326=EDGE_LOOP('',(#4168));
#1327=EDGE_LOOP('',(#4169));
#1328=EDGE_LOOP('',(#4170,#4171,#4172,#4173));
#1329=EDGE_LOOP('',(#4174,#4175,#4176,#4177));
#1330=EDGE_LOOP('',(#4178,#4179,#4180,#4181));
#1331=EDGE_LOOP('',(#4182));
#1332=EDGE_LOOP('',(#4183));
#1333=EDGE_LOOP('',(#4184,#4185,#4186,#4187));
#1334=EDGE_LOOP('',(#4188,#4189,#4190,#4191));
#1335=EDGE_LOOP('',(#4192,#4193,#4194,#4195));
#1336=EDGE_LOOP('',(#4196,#4197,#4198,#4199));
#1337=EDGE_LOOP('',(#4200));
#1338=EDGE_LOOP('',(#4201));
#1339=EDGE_LOOP('',(#4202,#4203,#4204,#4205));
#1340=EDGE_LOOP('',(#4206));
#1341=EDGE_LOOP('',(#4207));
#1342=EDGE_LOOP('',(#4208,#4209,#4210,#4211,#4212,#4213,#4214,#4215,#4216));
#1343=EDGE_LOOP('',(#4217,#4218,#4219,#4220,#4221,#4222,#4223,#4224,#4225));
#1344=EDGE_LOOP('',(#4226,#4227,#4228,#4229));
#1345=EDGE_LOOP('',(#4230,#4231,#4232,#4233));
#1346=EDGE_LOOP('',(#4234,#4235,#4236,#4237));
#1347=EDGE_LOOP('',(#4238,#4239,#4240,#4241));
#1348=EDGE_LOOP('',(#4242,#4243,#4244,#4245));
#1349=EDGE_LOOP('',(#4246,#4247,#4248,#4249));
#1350=EDGE_LOOP('',(#4250,#4251,#4252,#4253));
#1351=EDGE_LOOP('',(#4254));
#1352=EDGE_LOOP('',(#4255));
#1353=EDGE_LOOP('',(#4256));
#1354=EDGE_LOOP('',(#4257));
#1355=EDGE_LOOP('',(#4258,#4259,#4260,#4261));
#1356=EDGE_LOOP('',(#4262,#4263,#4264,#4265));
#1357=EDGE_LOOP('',(#4266));
#1358=EDGE_LOOP('',(#4267));
#1359=EDGE_LOOP('',(#4268));
#1360=EDGE_LOOP('',(#4269));
#1361=EDGE_LOOP('',(#4270));
#1362=EDGE_LOOP('',(#4271,#4272,#4273,#4274));
#1363=EDGE_LOOP('',(#4275,#4276,#4277,#4278));
#1364=EDGE_LOOP('',(#4279,#4280,#4281,#4282));
#1365=EDGE_LOOP('',(#4283));
#1366=EDGE_LOOP('',(#4284));
#1367=EDGE_LOOP('',(#4285,#4286,#4287,#4288));
#1368=EDGE_LOOP('',(#4289,#4290,#4291,#4292));
#1369=EDGE_LOOP('',(#4293,#4294,#4295,#4296));
#1370=EDGE_LOOP('',(#4297));
#1371=EDGE_LOOP('',(#4298,#4299,#4300,#4301));
#1372=EDGE_LOOP('',(#4302,#4303,#4304,#4305));
#1373=EDGE_LOOP('',(#4306,#4307,#4308,#4309));
#1374=EDGE_LOOP('',(#4310,#4311,#4312,#4313));
#1375=EDGE_LOOP('',(#4314,#4315,#4316,#4317));
#1376=EDGE_LOOP('',(#4318,#4319,#4320,#4321));
#1377=EDGE_LOOP('',(#4322,#4323,#4324,#4325,#4326,#4327));
#1378=EDGE_LOOP('',(#4328,#4329,#4330,#4331,#4332,#4333));
#1379=EDGE_LOOP('',(#4334,#4335,#4336,#4337));
#1380=EDGE_LOOP('',(#4338));
#1381=EDGE_LOOP('',(#4339));
#1382=EDGE_LOOP('',(#4340,#4341,#4342,#4343));
#1383=EDGE_LOOP('',(#4344,#4345,#4346,#4347));
#1384=EDGE_LOOP('',(#4348));
#1385=EDGE_LOOP('',(#4349));
#1386=EDGE_LOOP('',(#4350));
#1387=EDGE_LOOP('',(#4351));
#1388=EDGE_LOOP('',(#4352,#4353,#4354,#4355));
#1389=EDGE_LOOP('',(#4356,#4357,#4358,#4359,#4360,#4361,#4362,#4363));
#1390=EDGE_LOOP('',(#4364,#4365,#4366,#4367));
#1391=EDGE_LOOP('',(#4368,#4369,#4370,#4371,#4372,#4373));
#1392=EDGE_LOOP('',(#4374,#4375,#4376));
#1393=EDGE_LOOP('',(#4377,#4378,#4379,#4380,#4381));
#1394=EDGE_LOOP('',(#4382,#4383,#4384));
#1395=EDGE_LOOP('',(#4385,#4386,#4387,#4388,#4389));
#1396=EDGE_LOOP('',(#4390,#4391,#4392,#4393,#4394,#4395,#4396));
#1397=EDGE_LOOP('',(#4397,#4398,#4399,#4400,#4401,#4402,#4403,#4404,#4405,
#4406,#4407,#4408));
#1398=EDGE_LOOP('',(#4409,#4410));
#1399=EDGE_LOOP('',(#4411,#4412,#4413));
#1400=EDGE_LOOP('',(#4414,#4415,#4416));
#1401=EDGE_LOOP('',(#4417,#4418));
#1402=EDGE_LOOP('',(#4419,#4420,#4421,#4422,#4423,#4424));
#1403=EDGE_LOOP('',(#4425));
#1404=EDGE_LOOP('',(#4426));
#1405=EDGE_LOOP('',(#4427,#4428,#4429,#4430,#4431,#4432,#4433,#4434,#4435));
#1406=EDGE_LOOP('',(#4436));
#1407=EDGE_LOOP('',(#4437));
#1408=EDGE_LOOP('',(#4438));
#1409=EDGE_LOOP('',(#4439));
#1410=EDGE_LOOP('',(#4440,#4441,#4442,#4443));
#1411=EDGE_LOOP('',(#4444,#4445,#4446,#4447));
#1412=EDGE_LOOP('',(#4448));
#1413=EDGE_LOOP('',(#4449));
#1414=EDGE_LOOP('',(#4450));
#1415=EDGE_LOOP('',(#4451));
#1416=EDGE_LOOP('',(#4452,#4453,#4454,#4455));
#1417=EDGE_LOOP('',(#4456,#4457,#4458,#4459));
#1418=EDGE_LOOP('',(#4460));
#1419=EDGE_LOOP('',(#4461));
#1420=EDGE_LOOP('',(#4462));
#1421=EDGE_LOOP('',(#4463));
#1422=EDGE_LOOP('',(#4464,#4465,#4466,#4467));
#1423=EDGE_LOOP('',(#4468,#4469,#4470,#4471));
#1424=EDGE_LOOP('',(#4472));
#1425=EDGE_LOOP('',(#4473));
#1426=EDGE_LOOP('',(#4474));
#1427=EDGE_LOOP('',(#4475));
#1428=EDGE_LOOP('',(#4476,#4477,#4478,#4479,#4480,#4481));
#1429=EDGE_LOOP('',(#4482,#4483));
#1430=EDGE_LOOP('',(#4484,#4485,#4486,#4487));
#1431=EDGE_LOOP('',(#4488,#4489,#4490,#4491,#4492,#4493));
#1432=EDGE_LOOP('',(#4494));
#1433=EDGE_LOOP('',(#4495));
#1434=EDGE_LOOP('',(#4496,#4497,#4498,#4499));
#1435=EDGE_LOOP('',(#4500,#4501,#4502,#4503));
#1436=EDGE_LOOP('',(#4504));
#1437=EDGE_LOOP('',(#4505));
#1438=EDGE_LOOP('',(#4506,#4507,#4508,#4509));
#1439=EDGE_LOOP('',(#4510,#4511,#4512,#4513,#4514,#4515));
#1440=EDGE_LOOP('',(#4516));
#1441=EDGE_LOOP('',(#4517));
#1442=EDGE_LOOP('',(#4518,#4519,#4520,#4521));
#1443=EDGE_LOOP('',(#4522));
#1444=EDGE_LOOP('',(#4523));
#1445=EDGE_LOOP('',(#4524));
#1446=EDGE_LOOP('',(#4525));
#1447=EDGE_LOOP('',(#4526,#4527,#4528,#4529));
#1448=EDGE_LOOP('',(#4530));
#1449=EDGE_LOOP('',(#4531));
#1450=EDGE_LOOP('',(#4532,#4533,#4534,#4535,#4536,#4537));
#1451=EDGE_LOOP('',(#4538,#4539,#4540,#4541,#4542,#4543));
#1452=EDGE_LOOP('',(#4544));
#1453=EDGE_LOOP('',(#4545,#4546,#4547,#4548,#4549,#4550));
#1454=EDGE_LOOP('',(#4551));
#1455=EDGE_LOOP('',(#4552,#4553,#4554,#4555));
#1456=EDGE_LOOP('',(#4556,#4557,#4558,#4559));
#1457=EDGE_LOOP('',(#4560,#4561,#4562,#4563));
#1458=EDGE_LOOP('',(#4564,#4565,#4566,#4567));
#1459=EDGE_LOOP('',(#4568,#4569,#4570,#4571));
#1460=EDGE_LOOP('',(#4572,#4573,#4574,#4575));
#1461=EDGE_LOOP('',(#4576,#4577,#4578,#4579));
#1462=EDGE_LOOP('',(#4580));
#1463=EDGE_LOOP('',(#4581));
#1464=EDGE_LOOP('',(#4582,#4583,#4584,#4585));
#1465=EDGE_LOOP('',(#4586,#4587,#4588,#4589));
#1466=EDGE_LOOP('',(#4590,#4591,#4592,#4593));
#1467=EDGE_LOOP('',(#4594));
#1468=EDGE_LOOP('',(#4595));
#1469=EDGE_LOOP('',(#4596,#4597,#4598,#4599));
#1470=EDGE_LOOP('',(#4600,#4601,#4602,#4603));
#1471=EDGE_LOOP('',(#4604,#4605,#4606,#4607));
#1472=EDGE_LOOP('',(#4608,#4609,#4610,#4611));
#1473=EDGE_LOOP('',(#4612,#4613,#4614,#4615));
#1474=EDGE_LOOP('',(#4616));
#1475=EDGE_LOOP('',(#4617));
#1476=EDGE_LOOP('',(#4618));
#1477=EDGE_LOOP('',(#4619));
#1478=EDGE_LOOP('',(#4620));
#1479=EDGE_LOOP('',(#4621));
#1480=EDGE_LOOP('',(#4622,#4623,#4624,#4625));
#1481=EDGE_LOOP('',(#4626,#4627,#4628,#4629));
#1482=EDGE_LOOP('',(#4630,#4631,#4632,#4633));
#1483=EDGE_LOOP('',(#4634));
#1484=EDGE_LOOP('',(#4635));
#1485=EDGE_LOOP('',(#4636));
#1486=EDGE_LOOP('',(#4637));
#1487=EDGE_LOOP('',(#4638));
#1488=EDGE_LOOP('',(#4639));
#1489=EDGE_LOOP('',(#4640));
#1490=EDGE_LOOP('',(#4641));
#1491=EDGE_LOOP('',(#4642,#4643,#4644,#4645));
#1492=EDGE_LOOP('',(#4646,#4647,#4648,#4649));
#1493=EDGE_LOOP('',(#4650,#4651,#4652,#4653));
#1494=EDGE_LOOP('',(#4654,#4655,#4656,#4657));
#1495=EDGE_LOOP('',(#4658));
#1496=EDGE_LOOP('',(#4659));
#1497=EDGE_LOOP('',(#4660));
#1498=EDGE_LOOP('',(#4661));
#1499=EDGE_LOOP('',(#4662));
#1500=EDGE_LOOP('',(#4663));
#1501=EDGE_LOOP('',(#4664,#4665,#4666,#4667));
#1502=EDGE_LOOP('',(#4668,#4669,#4670,#4671));
#1503=EDGE_LOOP('',(#4672,#4673,#4674,#4675));
#1504=EDGE_LOOP('',(#4676));
#1505=EDGE_LOOP('',(#4677));
#1506=EDGE_LOOP('',(#4678));
#1507=EDGE_LOOP('',(#4679));
#1508=EDGE_LOOP('',(#4680));
#1509=EDGE_LOOP('',(#4681));
#1510=EDGE_LOOP('',(#4682));
#1511=EDGE_LOOP('',(#4683));
#1512=EDGE_LOOP('',(#4684));
#1513=EDGE_LOOP('',(#4685,#4686,#4687,#4688));
#1514=EDGE_LOOP('',(#4689,#4690,#4691,#4692));
#1515=EDGE_LOOP('',(#4693,#4694,#4695,#4696));
#1516=EDGE_LOOP('',(#4697));
#1517=EDGE_LOOP('',(#4698));
#1518=EDGE_LOOP('',(#4699,#4700,#4701,#4702));
#1519=EDGE_LOOP('',(#4703,#4704,#4705,#4706));
#1520=EDGE_LOOP('',(#4707,#4708,#4709,#4710));
#1521=EDGE_LOOP('',(#4711));
#1522=EDGE_LOOP('',(#4712,#4713,#4714,#4715));
#1523=EDGE_LOOP('',(#4716,#4717,#4718,#4719));
#1524=EDGE_LOOP('',(#4720,#4721,#4722,#4723));
#1525=EDGE_LOOP('',(#4724,#4725,#4726,#4727));
#1526=EDGE_LOOP('',(#4728,#4729,#4730,#4731));
#1527=EDGE_LOOP('',(#4732,#4733,#4734,#4735));
#1528=EDGE_LOOP('',(#4736,#4737,#4738,#4739,#4740,#4741));
#1529=EDGE_LOOP('',(#4742,#4743,#4744,#4745,#4746,#4747));
#1530=EDGE_LOOP('',(#4748,#4749,#4750,#4751));
#1531=EDGE_LOOP('',(#4752,#4753,#4754,#4755));
#1532=EDGE_LOOP('',(#4756));
#1533=EDGE_LOOP('',(#4757));
#1534=EDGE_LOOP('',(#4758));
#1535=EDGE_LOOP('',(#4759));
#1536=EDGE_LOOP('',(#4760,#4761,#4762,#4763,#4764,#4765,#4766,#4767,#4768));
#1537=EDGE_LOOP('',(#4769,#4770,#4771,#4772,#4773,#4774,#4775,#4776,#4777));
#1538=EDGE_LOOP('',(#4778,#4779,#4780,#4781));
#1539=EDGE_LOOP('',(#4782,#4783,#4784,#4785));
#1540=EDGE_LOOP('',(#4786,#4787,#4788,#4789));
#1541=EDGE_LOOP('',(#4790,#4791,#4792,#4793));
#1542=EDGE_LOOP('',(#4794,#4795,#4796,#4797));
#1543=EDGE_LOOP('',(#4798,#4799,#4800,#4801));
#1544=EDGE_LOOP('',(#4802,#4803,#4804,#4805));
#1545=EDGE_LOOP('',(#4806));
#1546=EDGE_LOOP('',(#4807));
#1547=EDGE_LOOP('',(#4808));
#1548=EDGE_LOOP('',(#4809));
#1549=EDGE_LOOP('',(#4810,#4811,#4812,#4813));
#1550=EDGE_LOOP('',(#4814,#4815,#4816,#4817,#4818));
#1551=EDGE_LOOP('',(#4819,#4820,#4821,#4822));
#1552=EDGE_LOOP('',(#4823,#4824,#4825,#4826));
#1553=EDGE_LOOP('',(#4827,#4828,#4829,#4830));
#1554=EDGE_LOOP('',(#4831,#4832,#4833,#4834));
#1555=EDGE_LOOP('',(#4835,#4836,#4837,#4838,#4839,#4840,#4841));
#1556=EDGE_LOOP('',(#4842));
#1557=EDGE_LOOP('',(#4843));
#1558=EDGE_LOOP('',(#4844,#4845,#4846,#4847));
#1559=EDGE_LOOP('',(#4848));
#1560=EDGE_LOOP('',(#4849,#4850,#4851));
#1561=EDGE_LOOP('',(#4852,#4853,#4854));
#1562=EDGE_LOOP('',(#4855,#4856,#4857));
#1563=EDGE_LOOP('',(#4858,#4859,#4860));
#1564=EDGE_LOOP('',(#4861,#4862,#4863,#4864,#4865,#4866));
#1565=EDGE_LOOP('',(#4867,#4868,#4869,#4870,#4871,#4872));
#1566=EDGE_LOOP('',(#4873,#4874,#4875,#4876,#4877,#4878));
#1567=EDGE_LOOP('',(#4879,#4880,#4881,#4882,#4883,#4884));
#1568=EDGE_LOOP('',(#4885,#4886,#4887,#4888));
#1569=EDGE_LOOP('',(#4889));
#1570=EDGE_LOOP('',(#4890,#4891));
#1571=EDGE_LOOP('',(#4892,#4893,#4894));
#1572=EDGE_LOOP('',(#4895,#4896));
#1573=EDGE_LOOP('',(#4897,#4898));
#1574=EDGE_LOOP('',(#4899,#4900,#4901,#4902));
#1575=EDGE_LOOP('',(#4903,#4904,#4905,#4906));
#1576=EDGE_LOOP('',(#4907,#4908,#4909,#4910));
#1577=EDGE_LOOP('',(#4911,#4912,#4913,#4914));
#1578=EDGE_LOOP('',(#4915,#4916,#4917,#4918));
#1579=EDGE_LOOP('',(#4919,#4920,#4921,#4922,#4923,#4924,#4925,#4926,#4927,
#4928,#4929,#4930));
#1580=EDGE_LOOP('',(#4931));
#1581=EDGE_LOOP('',(#4932,#4933,#4934,#4935));
#1582=EDGE_LOOP('',(#4936,#4937,#4938,#4939));
#1583=EDGE_LOOP('',(#4940,#4941,#4942,#4943));
#1584=EDGE_LOOP('',(#4944,#4945,#4946,#4947));
#1585=EDGE_LOOP('',(#4948,#4949,#4950,#4951));
#1586=EDGE_LOOP('',(#4952,#4953,#4954,#4955));
#1587=EDGE_LOOP('',(#4956,#4957,#4958,#4959));
#1588=EDGE_LOOP('',(#4960,#4961,#4962,#4963));
#1589=EDGE_LOOP('',(#4964,#4965,#4966,#4967));
#1590=EDGE_LOOP('',(#4968,#4969,#4970,#4971));
#1591=EDGE_LOOP('',(#4972,#4973,#4974,#4975));
#1592=EDGE_LOOP('',(#4976,#4977,#4978,#4979));
#1593=EDGE_LOOP('',(#4980,#4981,#4982,#4983));
#1594=EDGE_LOOP('',(#4984,#4985,#4986,#4987));
#1595=EDGE_LOOP('',(#4988,#4989,#4990,#4991));
#1596=EDGE_LOOP('',(#4992));
#1597=EDGE_LOOP('',(#4993));
#1598=EDGE_LOOP('',(#4994));
#1599=EDGE_LOOP('',(#4995));
#1600=EDGE_LOOP('',(#4996,#4997,#4998,#4999));
#1601=EDGE_LOOP('',(#5000,#5001,#5002,#5003));
#1602=EDGE_LOOP('',(#5004,#5005,#5006,#5007));
#1603=EDGE_LOOP('',(#5008,#5009,#5010,#5011));
#1604=EDGE_LOOP('',(#5012,#5013,#5014,#5015));
#1605=EDGE_LOOP('',(#5016,#5017,#5018,#5019));
#1606=EDGE_LOOP('',(#5020,#5021,#5022,#5023));
#1607=EDGE_LOOP('',(#5024,#5025,#5026,#5027));
#1608=EDGE_LOOP('',(#5028,#5029,#5030,#5031));
#1609=EDGE_LOOP('',(#5032,#5033,#5034,#5035));
#1610=EDGE_LOOP('',(#5036,#5037,#5038,#5039));
#1611=EDGE_LOOP('',(#5040,#5041,#5042,#5043));
#1612=EDGE_LOOP('',(#5044,#5045,#5046,#5047,#5048,#5049));
#1613=EDGE_LOOP('',(#5050,#5051,#5052,#5053,#5054,#5055));
#1614=EDGE_LOOP('',(#5056));
#1615=EDGE_LOOP('',(#5057));
#1616=EDGE_LOOP('',(#5058,#5059,#5060,#5061));
#1617=EDGE_LOOP('',(#5062,#5063,#5064,#5065));
#1618=EDGE_LOOP('',(#5066,#5067,#5068,#5069));
#1619=EDGE_LOOP('',(#5070));
#1620=EDGE_LOOP('',(#5071));
#1621=EDGE_LOOP('',(#5072,#5073,#5074,#5075));
#1622=EDGE_LOOP('',(#5076,#5077,#5078,#5079));
#1623=LINE('',#8431,#1999);
#1624=LINE('',#8438,#2000);
#1625=LINE('',#8445,#2001);
#1626=LINE('',#8451,#2002);
#1627=LINE('',#8457,#2003);
#1628=LINE('',#8463,#2004);
#1629=LINE('',#8468,#2005);
#1630=LINE('',#8472,#2006);
#1631=LINE('',#8476,#2007);
#1632=LINE('',#8479,#2008);
#1633=LINE('',#8482,#2009);
#1634=LINE('',#8484,#2010);
#1635=LINE('',#8486,#2011);
#1636=LINE('',#8488,#2012);
#1637=LINE('',#8489,#2013);
#1638=LINE('',#8494,#2014);
#1639=LINE('',#8500,#2015);
#1640=LINE('',#8510,#2016);
#1641=LINE('',#8512,#2017);
#1642=LINE('',#8513,#2018);
#1643=LINE('',#8516,#2019);
#1644=LINE('',#8517,#2020);
#1645=LINE('',#8520,#2021);
#1646=LINE('',#8521,#2022);
#1647=LINE('',#8523,#2023);
#1648=LINE('',#8530,#2024);
#1649=LINE('',#8537,#2025);
#1650=LINE('',#8544,#2026);
#1651=LINE('',#8550,#2027);
#1652=LINE('',#8556,#2028);
#1653=LINE('',#8562,#2029);
#1654=LINE('',#8567,#2030);
#1655=LINE('',#8571,#2031);
#1656=LINE('',#8575,#2032);
#1657=LINE('',#8578,#2033);
#1658=LINE('',#8581,#2034);
#1659=LINE('',#8583,#2035);
#1660=LINE('',#8585,#2036);
#1661=LINE('',#8587,#2037);
#1662=LINE('',#8588,#2038);
#1663=LINE('',#8593,#2039);
#1664=LINE('',#8599,#2040);
#1665=LINE('',#8610,#2041);
#1666=LINE('',#8611,#2042);
#1667=LINE('',#8612,#2043);
#1668=LINE('',#8615,#2044);
#1669=LINE('',#8616,#2045);
#1670=LINE('',#8619,#2046);
#1671=LINE('',#8620,#2047);
#1672=LINE('',#8622,#2048);
#1673=LINE('',#8629,#2049);
#1674=LINE('',#8635,#2050);
#1675=LINE('',#8641,#2051);
#1676=LINE('',#8647,#2052);
#1677=LINE('',#8652,#2053);
#1678=LINE('',#8654,#2054);
#1679=LINE('',#8656,#2055);
#1680=LINE('',#8657,#2056);
#1681=LINE('',#8661,#2057);
#1682=LINE('',#8663,#2058);
#1683=LINE('',#8665,#2059);
#1684=LINE('',#8666,#2060);
#1685=LINE('',#8669,#2061);
#1686=LINE('',#8671,#2062);
#1687=LINE('',#8672,#2063);
#1688=LINE('',#8675,#2064);
#1689=LINE('',#8677,#2065);
#1690=LINE('',#8678,#2066);
#1691=LINE('',#8682,#2067);
#1692=LINE('',#8684,#2068);
#1693=LINE('',#8686,#2069);
#1694=LINE('',#8688,#2070);
#1695=LINE('',#8689,#2071);
#1696=LINE('',#8692,#2072);
#1697=LINE('',#8693,#2073);
#1698=LINE('',#8696,#2074);
#1699=LINE('',#8697,#2075);
#1700=LINE('',#8702,#2076);
#1701=LINE('',#8703,#2077);
#1702=LINE('',#8706,#2078);
#1703=LINE('',#8707,#2079);
#1704=LINE('',#8709,#2080);
#1705=LINE('',#8720,#2081);
#1706=LINE('',#8726,#2082);
#1707=LINE('',#8730,#2083);
#1708=LINE('',#8743,#2084);
#1709=LINE('',#8751,#2085);
#1710=LINE('',#8756,#2086);
#1711=LINE('',#8765,#2087);
#1712=LINE('',#8772,#2088);
#1713=LINE('',#8779,#2089);
#1714=LINE('',#8785,#2090);
#1715=LINE('',#8791,#2091);
#1716=LINE('',#8797,#2092);
#1717=LINE('',#8803,#2093);
#1718=LINE('',#8808,#2094);
#1719=LINE('',#8810,#2095);
#1720=LINE('',#8812,#2096);
#1721=LINE('',#8813,#2097);
#1722=LINE('',#8816,#2098);
#1723=LINE('',#8818,#2099);
#1724=LINE('',#8819,#2100);
#1725=LINE('',#8822,#2101);
#1726=LINE('',#8824,#2102);
#1727=LINE('',#8825,#2103);
#1728=LINE('',#8827,#2104);
#1729=LINE('',#8828,#2105);
#1730=LINE('',#8839,#2106);
#1731=LINE('',#8845,#2107);
#1732=LINE('',#8853,#2108);
#1733=LINE('',#8855,#2109);
#1734=LINE('',#8857,#2110);
#1735=LINE('',#8858,#2111);
#1736=LINE('',#8861,#2112);
#1737=LINE('',#8863,#2113);
#1738=LINE('',#8864,#2114);
#1739=LINE('',#8867,#2115);
#1740=LINE('',#8869,#2116);
#1741=LINE('',#8870,#2117);
#1742=LINE('',#8873,#2118);
#1743=LINE('',#8875,#2119);
#1744=LINE('',#8876,#2120);
#1745=LINE('',#8879,#2121);
#1746=LINE('',#8881,#2122);
#1747=LINE('',#8882,#2123);
#1748=LINE('',#8884,#2124);
#1749=LINE('',#8885,#2125);
#1750=LINE('',#8895,#2126);
#1751=LINE('',#8904,#2127);
#1752=LINE('',#8908,#2128);
#1753=LINE('',#8912,#2129);
#1754=LINE('',#8919,#2130);
#1755=LINE('',#8921,#2131);
#1756=LINE('',#8927,#2132);
#1757=LINE('',#8931,#2133);
#1758=LINE('',#8938,#2134);
#1759=LINE('',#8953,#2135);
#1760=LINE('',#8974,#2136);
#1761=LINE('',#8999,#2137);
#1762=LINE('',#9000,#2138);
#1763=LINE('',#9002,#2139);
#1764=LINE('',#9004,#2140);
#1765=LINE('',#9009,#2141);
#1766=LINE('',#9012,#2142);
#1767=LINE('',#9014,#2143);
#1768=LINE('',#9023,#2144);
#1769=LINE('',#9029,#2145);
#1770=LINE('',#9040,#2146);
#1771=LINE('',#9044,#2147);
#1772=LINE('',#9048,#2148);
#1773=LINE('',#9055,#2149);
#1774=LINE('',#9059,#2150);
#1775=LINE('',#9063,#2151);
#1776=LINE('',#9068,#2152);
#1777=LINE('',#9070,#2153);
#1778=LINE('',#9072,#2154);
#1779=LINE('',#9073,#2155);
#1780=LINE('',#9076,#2156);
#1781=LINE('',#9078,#2157);
#1782=LINE('',#9079,#2158);
#1783=LINE('',#9082,#2159);
#1784=LINE('',#9084,#2160);
#1785=LINE('',#9085,#2161);
#1786=LINE('',#9088,#2162);
#1787=LINE('',#9090,#2163);
#1788=LINE('',#9091,#2164);
#1789=LINE('',#9094,#2165);
#1790=LINE('',#9096,#2166);
#1791=LINE('',#9097,#2167);
#1792=LINE('',#9099,#2168);
#1793=LINE('',#9100,#2169);
#1794=LINE('',#9108,#2170);
#1795=LINE('',#9152,#2171);
#1796=LINE('',#9158,#2172);
#1797=LINE('',#9166,#2173);
#1798=LINE('',#9170,#2174);
#1799=LINE('',#9176,#2175);
#1800=LINE('',#9185,#2176);
#1801=LINE('',#9188,#2177);
#1802=LINE('',#9193,#2178);
#1803=LINE('',#9214,#2179);
#1804=LINE('',#9219,#2180);
#1805=LINE('',#9224,#2181);
#1806=LINE('',#9239,#2182);
#1807=LINE('',#9246,#2183);
#1808=LINE('',#9248,#2184);
#1809=LINE('',#9257,#2185);
#1810=LINE('',#9263,#2186);
#1811=LINE('',#9272,#2187);
#1812=LINE('',#9278,#2188);
#1813=LINE('',#9287,#2189);
#1814=LINE('',#9293,#2190);
#1815=LINE('',#9305,#2191);
#1816=LINE('',#9317,#2192);
#1817=LINE('',#9325,#2193);
#1818=LINE('',#9330,#2194);
#1819=LINE('',#9345,#2195);
#1820=LINE('',#9353,#2196);
#1821=LINE('',#9363,#2197);
#1822=LINE('',#9366,#2198);
#1823=LINE('',#9371,#2199);
#1824=LINE('',#9373,#2200);
#1825=LINE('',#9375,#2201);
#1826=LINE('',#9377,#2202);
#1827=LINE('',#9379,#2203);
#1828=LINE('',#9380,#2204);
#1829=LINE('',#9386,#2205);
#1830=LINE('',#9388,#2206);
#1831=LINE('',#9390,#2207);
#1832=LINE('',#9392,#2208);
#1833=LINE('',#9394,#2209);
#1834=LINE('',#9395,#2210);
#1835=LINE('',#9399,#2211);
#1836=LINE('',#9400,#2212);
#1837=LINE('',#9402,#2213);
#1838=LINE('',#9404,#2214);
#1839=LINE('',#9406,#2215);
#1840=LINE('',#9408,#2216);
#1841=LINE('',#9412,#2217);
#1842=LINE('',#9420,#2218);
#1843=LINE('',#9424,#2219);
#1844=LINE('',#9428,#2220);
#1845=LINE('',#9433,#2221);
#1846=LINE('',#9439,#2222);
#1847=LINE('',#9445,#2223);
#1848=LINE('',#9451,#2224);
#1849=LINE('',#9457,#2225);
#1850=LINE('',#9467,#2226);
#1851=LINE('',#9472,#2227);
#1852=LINE('',#9476,#2228);
#1853=LINE('',#9485,#2229);
#1854=LINE('',#9491,#2230);
#1855=LINE('',#9497,#2231);
#1856=LINE('',#9503,#2232);
#1857=LINE('',#9512,#2233);
#1858=LINE('',#9518,#2234);
#1859=LINE('',#9523,#2235);
#1860=LINE('',#9533,#2236);
#1861=LINE('',#9537,#2237);
#1862=LINE('',#9541,#2238);
#1863=LINE('',#9548,#2239);
#1864=LINE('',#9552,#2240);
#1865=LINE('',#9556,#2241);
#1866=LINE('',#9561,#2242);
#1867=LINE('',#9563,#2243);
#1868=LINE('',#9565,#2244);
#1869=LINE('',#9566,#2245);
#1870=LINE('',#9569,#2246);
#1871=LINE('',#9571,#2247);
#1872=LINE('',#9572,#2248);
#1873=LINE('',#9575,#2249);
#1874=LINE('',#9577,#2250);
#1875=LINE('',#9578,#2251);
#1876=LINE('',#9581,#2252);
#1877=LINE('',#9583,#2253);
#1878=LINE('',#9584,#2254);
#1879=LINE('',#9587,#2255);
#1880=LINE('',#9589,#2256);
#1881=LINE('',#9590,#2257);
#1882=LINE('',#9592,#2258);
#1883=LINE('',#9593,#2259);
#1884=LINE('',#9601,#2260);
#1885=LINE('',#9607,#2261);
#1886=LINE('',#9623,#2262);
#1887=LINE('',#9644,#2263);
#1888=LINE('',#9669,#2264);
#1889=LINE('',#9670,#2265);
#1890=LINE('',#9672,#2266);
#1891=LINE('',#9674,#2267);
#1892=LINE('',#9679,#2268);
#1893=LINE('',#9682,#2269);
#1894=LINE('',#9684,#2270);
#1895=LINE('',#9727,#2271);
#1896=LINE('',#9729,#2272);
#1897=LINE('',#9730,#2273);
#1898=LINE('',#9735,#2274);
#1899=LINE('',#9737,#2275);
#1900=LINE('',#9743,#2276);
#1901=LINE('',#9744,#2277);
#1902=LINE('',#9747,#2278);
#1903=LINE('',#9753,#2279);
#1904=LINE('',#9763,#2280);
#1905=LINE('',#9771,#2281);
#1906=LINE('',#9772,#2282);
#1907=LINE('',#9778,#2283);
#1908=LINE('',#9779,#2284);
#1909=LINE('',#9785,#2285);
#1910=LINE('',#9786,#2286);
#1911=LINE('',#9792,#2287);
#1912=LINE('',#9793,#2288);
#1913=LINE('',#9795,#2289);
#1914=LINE('',#9797,#2290);
#1915=LINE('',#9799,#2291);
#1916=LINE('',#9800,#2292);
#1917=LINE('',#9802,#2293);
#1918=LINE('',#9804,#2294);
#1919=LINE('',#9805,#2295);
#1920=LINE('',#9807,#2296);
#1921=LINE('',#9809,#2297);
#1922=LINE('',#9810,#2298);
#1923=LINE('',#9812,#2299);
#1924=LINE('',#9813,#2300);
#1925=LINE('',#9828,#2301);
#1926=LINE('',#9830,#2302);
#1927=LINE('',#9832,#2303);
#1928=LINE('',#9833,#2304);
#1929=LINE('',#9836,#2305);
#1930=LINE('',#9838,#2306);
#1931=LINE('',#9839,#2307);
#1932=LINE('',#9842,#2308);
#1933=LINE('',#9844,#2309);
#1934=LINE('',#9845,#2310);
#1935=LINE('',#9847,#2311);
#1936=LINE('',#9848,#2312);
#1937=LINE('',#9852,#2313);
#1938=LINE('',#9859,#2314);
#1939=LINE('',#9861,#2315);
#1940=LINE('',#9863,#2316);
#1941=LINE('',#9864,#2317);
#1942=LINE('',#9867,#2318);
#1943=LINE('',#9869,#2319);
#1944=LINE('',#9870,#2320);
#1945=LINE('',#9873,#2321);
#1946=LINE('',#9875,#2322);
#1947=LINE('',#9876,#2323);
#1948=LINE('',#9878,#2324);
#1949=LINE('',#9879,#2325);
#1950=LINE('',#9883,#2326);
#1951=LINE('',#9885,#2327);
#1952=LINE('',#9887,#2328);
#1953=LINE('',#9888,#2329);
#1954=LINE('',#9891,#2330);
#1955=LINE('',#9893,#2331);
#1956=LINE('',#9894,#2332);
#1957=LINE('',#9897,#2333);
#1958=LINE('',#9899,#2334);
#1959=LINE('',#9900,#2335);
#1960=LINE('',#9902,#2336);
#1961=LINE('',#9903,#2337);
#1962=LINE('',#9911,#2338);
#1963=LINE('',#9917,#2339);
#1964=LINE('',#9925,#2340);
#1965=LINE('',#9927,#2341);
#1966=LINE('',#9929,#2342);
#1967=LINE('',#9930,#2343);
#1968=LINE('',#9933,#2344);
#1969=LINE('',#9935,#2345);
#1970=LINE('',#9936,#2346);
#1971=LINE('',#9939,#2347);
#1972=LINE('',#9941,#2348);
#1973=LINE('',#9942,#2349);
#1974=LINE('',#9944,#2350);
#1975=LINE('',#9945,#2351);
#1976=LINE('',#9952,#2352);
#1977=LINE('',#9954,#2353);
#1978=LINE('',#9956,#2354);
#1979=LINE('',#9957,#2355);
#1980=LINE('',#9960,#2356);
#1981=LINE('',#9962,#2357);
#1982=LINE('',#9963,#2358);
#1983=LINE('',#9966,#2359);
#1984=LINE('',#9968,#2360);
#1985=LINE('',#9969,#2361);
#1986=LINE('',#9972,#2362);
#1987=LINE('',#9974,#2363);
#1988=LINE('',#9975,#2364);
#1989=LINE('',#9978,#2365);
#1990=LINE('',#9980,#2366);
#1991=LINE('',#9981,#2367);
#1992=LINE('',#9983,#2368);
#1993=LINE('',#9984,#2369);
#1994=LINE('',#9996,#2370);
#1995=LINE('',#10000,#2371);
#1996=LINE('',#10004,#2372);
#1997=LINE('',#10011,#2373);
#1998=LINE('',#10013,#2374);
#1999=VECTOR('',#6631,0.165);
#2000=VECTOR('',#6640,0.165);
#2001=VECTOR('',#6649,0.275);
#2002=VECTOR('',#6656,0.275);
#2003=VECTOR('',#6663,0.275);
#2004=VECTOR('',#6670,0.275);
#2005=VECTOR('',#6675,1.);
#2006=VECTOR('',#6678,1.);
#2007=VECTOR('',#6683,1.);
#2008=VECTOR('',#6686,1.);
#2009=VECTOR('',#6689,1.);
#2010=VECTOR('',#6690,1.);
#2011=VECTOR('',#6691,1.);
#2012=VECTOR('',#6692,1.);
#2013=VECTOR('',#6693,1.);
#2014=VECTOR('',#6698,0.93);
#2015=VECTOR('',#6705,1.3);
#2016=VECTOR('',#6720,1.);
#2017=VECTOR('',#6721,1.);
#2018=VECTOR('',#6722,1.);
#2019=VECTOR('',#6725,1.);
#2020=VECTOR('',#6726,1.);
#2021=VECTOR('',#6729,1.);
#2022=VECTOR('',#6730,1.);
#2023=VECTOR('',#6733,1.);
#2024=VECTOR('',#6742,0.165);
#2025=VECTOR('',#6751,0.165);
#2026=VECTOR('',#6760,0.275);
#2027=VECTOR('',#6767,0.275);
#2028=VECTOR('',#6774,0.275);
#2029=VECTOR('',#6781,0.275);
#2030=VECTOR('',#6786,1.);
#2031=VECTOR('',#6789,1.);
#2032=VECTOR('',#6794,1.);
#2033=VECTOR('',#6797,1.);
#2034=VECTOR('',#6800,1.);
#2035=VECTOR('',#6801,1.);
#2036=VECTOR('',#6802,1.);
#2037=VECTOR('',#6803,1.);
#2038=VECTOR('',#6804,1.);
#2039=VECTOR('',#6809,0.93);
#2040=VECTOR('',#6816,1.3);
#2041=VECTOR('',#6831,1.);
#2042=VECTOR('',#6832,1.);
#2043=VECTOR('',#6833,1.);
#2044=VECTOR('',#6836,1.);
#2045=VECTOR('',#6837,1.);
#2046=VECTOR('',#6840,1.);
#2047=VECTOR('',#6841,1.);
#2048=VECTOR('',#6844,1.);
#2049=VECTOR('',#6853,0.275);
#2050=VECTOR('',#6860,0.275);
#2051=VECTOR('',#6867,0.275);
#2052=VECTOR('',#6874,0.275);
#2053=VECTOR('',#6879,1.);
#2054=VECTOR('',#6880,1.);
#2055=VECTOR('',#6881,1.);
#2056=VECTOR('',#6882,1.);
#2057=VECTOR('',#6885,1.);
#2058=VECTOR('',#6886,1.);
#2059=VECTOR('',#6887,1.);
#2060=VECTOR('',#6888,1.);
#2061=VECTOR('',#6891,1.);
#2062=VECTOR('',#6892,1.);
#2063=VECTOR('',#6893,1.);
#2064=VECTOR('',#6896,1.);
#2065=VECTOR('',#6897,1.);
#2066=VECTOR('',#6898,1.);
#2067=VECTOR('',#6903,1.);
#2068=VECTOR('',#6904,1.);
#2069=VECTOR('',#6905,1.);
#2070=VECTOR('',#6906,1.);
#2071=VECTOR('',#6907,1.);
#2072=VECTOR('',#6910,1.);
#2073=VECTOR('',#6911,1.);
#2074=VECTOR('',#6914,1.);
#2075=VECTOR('',#6915,1.);
#2076=VECTOR('',#6922,1.);
#2077=VECTOR('',#6923,1.);
#2078=VECTOR('',#6926,1.);
#2079=VECTOR('',#6927,1.);
#2080=VECTOR('',#6930,1.);
#2081=VECTOR('',#6945,1.2);
#2082=VECTOR('',#6952,0.405);
#2083=VECTOR('',#6957,0.7);
#2084=VECTOR('',#6976,0.61);
#2085=VECTOR('',#6987,0.405);
#2086=VECTOR('',#6992,1.);
#2087=VECTOR('',#7005,0.3);
#2088=VECTOR('',#7014,0.3);
#2089=VECTOR('',#7023,0.225);
#2090=VECTOR('',#7030,0.225);
#2091=VECTOR('',#7037,0.225);
#2092=VECTOR('',#7044,0.225);
#2093=VECTOR('',#7051,1.01);
#2094=VECTOR('',#7056,1.);
#2095=VECTOR('',#7057,1.);
#2096=VECTOR('',#7058,1.);
#2097=VECTOR('',#7059,1.);
#2098=VECTOR('',#7062,1.);
#2099=VECTOR('',#7063,1.);
#2100=VECTOR('',#7064,1.);
#2101=VECTOR('',#7067,1.);
#2102=VECTOR('',#7068,1.);
#2103=VECTOR('',#7069,1.);
#2104=VECTOR('',#7072,1.);
#2105=VECTOR('',#7073,1.);
#2106=VECTOR('',#7088,0.75);
#2107=VECTOR('',#7095,1.3);
#2108=VECTOR('',#7106,1.);
#2109=VECTOR('',#7107,1.);
#2110=VECTOR('',#7108,1.);
#2111=VECTOR('',#7109,1.);
#2112=VECTOR('',#7112,1.);
#2113=VECTOR('',#7113,1.);
#2114=VECTOR('',#7114,1.);
#2115=VECTOR('',#7117,1.);
#2116=VECTOR('',#7118,1.);
#2117=VECTOR('',#7119,1.);
#2118=VECTOR('',#7122,1.);
#2119=VECTOR('',#7123,1.);
#2120=VECTOR('',#7124,1.);
#2121=VECTOR('',#7127,1.);
#2122=VECTOR('',#7128,1.);
#2123=VECTOR('',#7129,1.);
#2124=VECTOR('',#7132,1.);
#2125=VECTOR('',#7133,1.);
#2126=VECTOR('',#7146,0.25);
#2127=VECTOR('',#7159,0.4);
#2128=VECTOR('',#7164,0.425);
#2129=VECTOR('',#7169,0.41);
#2130=VECTOR('',#7178,0.26);
#2131=VECTOR('',#7181,0.25);
#2132=VECTOR('',#7188,0.275);
#2133=VECTOR('',#7193,0.265);
#2134=VECTOR('',#7202,0.5);
#2135=VECTOR('',#7211,0.47094010767585);
#2136=VECTOR('',#7218,0.47094010767585);
#2137=VECTOR('',#7221,1.);
#2138=VECTOR('',#7222,1.);
#2139=VECTOR('',#7225,1.);
#2140=VECTOR('',#7228,1.);
#2141=VECTOR('',#7233,0.25);
#2142=VECTOR('',#7238,1.);
#2143=VECTOR('',#7241,1.);
#2144=VECTOR('',#7254,0.225);
#2145=VECTOR('',#7261,0.4);
#2146=VECTOR('',#7278,0.325);
#2147=VECTOR('',#7283,0.35);
#2148=VECTOR('',#7288,0.335);
#2149=VECTOR('',#7297,0.21);
#2150=VECTOR('',#7302,0.2);
#2151=VECTOR('',#7307,0.18);
#2152=VECTOR('',#7312,1.);
#2153=VECTOR('',#7313,1.);
#2154=VECTOR('',#7314,1.);
#2155=VECTOR('',#7315,1.);
#2156=VECTOR('',#7318,1.);
#2157=VECTOR('',#7319,1.);
#2158=VECTOR('',#7320,1.);
#2159=VECTOR('',#7323,1.);
#2160=VECTOR('',#7324,1.);
#2161=VECTOR('',#7325,1.);
#2162=VECTOR('',#7328,1.);
#2163=VECTOR('',#7329,1.);
#2164=VECTOR('',#7330,1.);
#2165=VECTOR('',#7333,1.);
#2166=VECTOR('',#7334,1.);
#2167=VECTOR('',#7335,1.);
#2168=VECTOR('',#7338,1.);
#2169=VECTOR('',#7339,1.);
#2170=VECTOR('',#7350,0.3);
#2171=VECTOR('',#7433,0.79);
#2172=VECTOR('',#7440,2.2);
#2173=VECTOR('',#7451,1.);
#2174=VECTOR('',#7454,1.);
#2175=VECTOR('',#7461,0.93);
#2176=VECTOR('',#7472,1.);
#2177=VECTOR('',#7475,1.);
#2178=VECTOR('',#7480,0.93);
#2179=VECTOR('',#7513,0.93);
#2180=VECTOR('',#7518,1.);
#2181=VECTOR('',#7523,1.);
#2182=VECTOR('',#7544,1.6);
#2183=VECTOR('',#7555,1.6);
#2184=VECTOR('',#7556,1.6);
#2185=VECTOR('',#7569,0.79);
#2186=VECTOR('',#7576,1.065);
#2187=VECTOR('',#7589,0.789999999999999);
#2188=VECTOR('',#7596,1.065);
#2189=VECTOR('',#7609,0.79);
#2190=VECTOR('',#7616,1.065);
#2191=VECTOR('',#7631,0.79);
#2192=VECTOR('',#7646,0.79);
#2193=VECTOR('',#7657,0.93);
#2194=VECTOR('',#7662,0.93);
#2195=VECTOR('',#7681,1.2);
#2196=VECTOR('',#7692,1.45);
#2197=VECTOR('',#7705,1.45);
#2198=VECTOR('',#7710,1.2);
#2199=VECTOR('',#7715,1.);
#2200=VECTOR('',#7716,1.);
#2201=VECTOR('',#7717,1.);
#2202=VECTOR('',#7718,1.);
#2203=VECTOR('',#7719,1.);
#2204=VECTOR('',#7720,1.);
#2205=VECTOR('',#7725,1.);
#2206=VECTOR('',#7726,1.);
#2207=VECTOR('',#7727,1.);
#2208=VECTOR('',#7728,1.);
#2209=VECTOR('',#7729,1.);
#2210=VECTOR('',#7730,1.);
#2211=VECTOR('',#7735,1.);
#2212=VECTOR('',#7736,1.);
#2213=VECTOR('',#7739,1.);
#2214=VECTOR('',#7742,1.);
#2215=VECTOR('',#7745,1.);
#2216=VECTOR('',#7748,1.);
#2217=VECTOR('',#7753,1.065);
#2218=VECTOR('',#7764,1.025);
#2219=VECTOR('',#7769,1.065);
#2220=VECTOR('',#7774,1.025);
#2221=VECTOR('',#7781,0.79);
#2222=VECTOR('',#7788,0.44);
#2223=VECTOR('',#7795,0.44);
#2224=VECTOR('',#7802,0.44);
#2225=VECTOR('',#7809,0.44);
#2226=VECTOR('',#7822,3.5);
#2227=VECTOR('',#7827,0.79);
#2228=VECTOR('',#7832,1.5);
#2229=VECTOR('',#7845,0.44);
#2230=VECTOR('',#7852,0.44);
#2231=VECTOR('',#7859,0.44);
#2232=VECTOR('',#7866,0.44);
#2233=VECTOR('',#7877,3.5);
#2234=VECTOR('',#7884,0.79);
#2235=VECTOR('',#7891,1.5);
#2236=VECTOR('',#7906,0.625);
#2237=VECTOR('',#7911,0.65);
#2238=VECTOR('',#7916,0.635);
#2239=VECTOR('',#7925,0.41);
#2240=VECTOR('',#7930,0.4);
#2241=VECTOR('',#7935,0.36);
#2242=VECTOR('',#7940,1.);
#2243=VECTOR('',#7941,1.);
#2244=VECTOR('',#7942,1.);
#2245=VECTOR('',#7943,1.);
#2246=VECTOR('',#7946,1.);
#2247=VECTOR('',#7947,1.);
#2248=VECTOR('',#7948,1.);
#2249=VECTOR('',#7951,1.);
#2250=VECTOR('',#7952,1.);
#2251=VECTOR('',#7953,1.);
#2252=VECTOR('',#7956,1.);
#2253=VECTOR('',#7957,1.);
#2254=VECTOR('',#7958,1.);
#2255=VECTOR('',#7961,1.);
#2256=VECTOR('',#7962,1.);
#2257=VECTOR('',#7963,1.);
#2258=VECTOR('',#7966,1.);
#2259=VECTOR('',#7967,1.);
#2260=VECTOR('',#7978,0.42);
#2261=VECTOR('',#7985,0.8);
#2262=VECTOR('',#7996,0.734027674973257);
#2263=VECTOR('',#8003,0.734027674973257);
#2264=VECTOR('',#8006,1.);
#2265=VECTOR('',#8007,1.);
#2266=VECTOR('',#8010,1.);
#2267=VECTOR('',#8013,1.);
#2268=VECTOR('',#8018,0.4);
#2269=VECTOR('',#8023,1.);
#2270=VECTOR('',#8026,1.);
#2271=VECTOR('',#8105,1.);
#2272=VECTOR('',#8106,1.);
#2273=VECTOR('',#8107,1.);
#2274=VECTOR('',#8112,1.);
#2275=VECTOR('',#8113,1.);
#2276=VECTOR('',#8120,1.);
#2277=VECTOR('',#8121,1.);
#2278=VECTOR('',#8126,1.);
#2279=VECTOR('',#8133,0.75);
#2280=VECTOR('',#8146,0.165);
#2281=VECTOR('',#8155,1.);
#2282=VECTOR('',#8156,1.);
#2283=VECTOR('',#8161,1.);
#2284=VECTOR('',#8162,1.);
#2285=VECTOR('',#8167,1.);
#2286=VECTOR('',#8168,1.);
#2287=VECTOR('',#8173,1.);
#2288=VECTOR('',#8174,1.);
#2289=VECTOR('',#8177,1.);
#2290=VECTOR('',#8178,1.);
#2291=VECTOR('',#8179,1.);
#2292=VECTOR('',#8180,1.);
#2293=VECTOR('',#8183,1.);
#2294=VECTOR('',#8184,1.);
#2295=VECTOR('',#8185,1.);
#2296=VECTOR('',#8188,1.);
#2297=VECTOR('',#8189,1.);
#2298=VECTOR('',#8190,1.);
#2299=VECTOR('',#8193,1.);
#2300=VECTOR('',#8194,1.);
#2301=VECTOR('',#8217,1.);
#2302=VECTOR('',#8218,1.);
#2303=VECTOR('',#8219,1.);
#2304=VECTOR('',#8220,1.);
#2305=VECTOR('',#8223,1.);
#2306=VECTOR('',#8224,1.);
#2307=VECTOR('',#8225,1.);
#2308=VECTOR('',#8228,1.);
#2309=VECTOR('',#8229,1.);
#2310=VECTOR('',#8230,1.);
#2311=VECTOR('',#8233,1.);
#2312=VECTOR('',#8234,1.);
#2313=VECTOR('',#8239,0.4);
#2314=VECTOR('',#8248,1.);
#2315=VECTOR('',#8249,1.);
#2316=VECTOR('',#8250,1.);
#2317=VECTOR('',#8251,1.);
#2318=VECTOR('',#8254,1.);
#2319=VECTOR('',#8255,1.);
#2320=VECTOR('',#8256,1.);
#2321=VECTOR('',#8259,1.);
#2322=VECTOR('',#8260,1.);
#2323=VECTOR('',#8261,1.);
#2324=VECTOR('',#8264,1.);
#2325=VECTOR('',#8265,1.);
#2326=VECTOR('',#8268,1.);
#2327=VECTOR('',#8269,1.);
#2328=VECTOR('',#8270,1.);
#2329=VECTOR('',#8271,1.);
#2330=VECTOR('',#8274,1.);
#2331=VECTOR('',#8275,1.);
#2332=VECTOR('',#8276,1.);
#2333=VECTOR('',#8279,1.);
#2334=VECTOR('',#8280,1.);
#2335=VECTOR('',#8281,1.);
#2336=VECTOR('',#8284,1.);
#2337=VECTOR('',#8285,1.);
#2338=VECTOR('',#8296,0.225);
#2339=VECTOR('',#8303,0.6);
#2340=VECTOR('',#8314,1.);
#2341=VECTOR('',#8315,1.);
#2342=VECTOR('',#8316,1.);
#2343=VECTOR('',#8317,1.);
#2344=VECTOR('',#8320,1.);
#2345=VECTOR('',#8321,1.);
#2346=VECTOR('',#8322,1.);
#2347=VECTOR('',#8325,1.);
#2348=VECTOR('',#8326,1.);
#2349=VECTOR('',#8327,1.);
#2350=VECTOR('',#8330,1.);
#2351=VECTOR('',#8331,1.);
#2352=VECTOR('',#8340,1.);
#2353=VECTOR('',#8341,1.);
#2354=VECTOR('',#8342,1.);
#2355=VECTOR('',#8343,1.);
#2356=VECTOR('',#8346,1.);
#2357=VECTOR('',#8347,1.);
#2358=VECTOR('',#8348,1.);
#2359=VECTOR('',#8351,1.);
#2360=VECTOR('',#8352,1.);
#2361=VECTOR('',#8353,1.);
#2362=VECTOR('',#8356,1.);
#2363=VECTOR('',#8357,1.);
#2364=VECTOR('',#8358,1.);
#2365=VECTOR('',#8361,1.);
#2366=VECTOR('',#8362,1.);
#2367=VECTOR('',#8363,1.);
#2368=VECTOR('',#8366,1.);
#2369=VECTOR('',#8367,1.);
#2370=VECTOR('',#8384,0.325);
#2371=VECTOR('',#8389,0.35);
#2372=VECTOR('',#8394,0.335);
#2373=VECTOR('',#8403,0.21);
#2374=VECTOR('',#8406,0.2);
#2375=CIRCLE('',#5910,0.165);
#2376=CIRCLE('',#5911,0.165);
#2377=CIRCLE('',#5914,0.165);
#2378=CIRCLE('',#5915,0.165);
#2379=CIRCLE('',#5918,0.275);
#2380=CIRCLE('',#5919,0.275);
#2381=CIRCLE('',#5921,0.275);
#2382=CIRCLE('',#5922,0.275);
#2383=CIRCLE('',#5924,0.275);
#2384=CIRCLE('',#5925,0.275);
#2385=CIRCLE('',#5927,0.275);
#2386=CIRCLE('',#5928,0.275);
#2387=CIRCLE('',#5930,0.7);
#2388=CIRCLE('',#5931,0.7);
#2389=CIRCLE('',#5933,0.556776436283003);
#2390=CIRCLE('',#5936,0.93);
#2391=CIRCLE('',#5937,0.93);
#2392=CIRCLE('',#5939,1.3);
#2393=CIRCLE('',#5940,1.3);
#2394=CIRCLE('',#5942,1.24899959967968);
#2395=CIRCLE('',#5945,1.59980467557762);
#2396=CIRCLE('',#5953,0.165);
#2397=CIRCLE('',#5954,0.165);
#2398=CIRCLE('',#5957,0.165);
#2399=CIRCLE('',#5958,0.165);
#2400=CIRCLE('',#5961,0.275);
#2401=CIRCLE('',#5962,0.275);
#2402=CIRCLE('',#5964,0.275);
#2403=CIRCLE('',#5965,0.275);
#2404=CIRCLE('',#5967,0.275);
#2405=CIRCLE('',#5968,0.275);
#2406=CIRCLE('',#5970,0.275);
#2407=CIRCLE('',#5971,0.275);
#2408=CIRCLE('',#5973,0.7);
#2409=CIRCLE('',#5974,0.7);
#2410=CIRCLE('',#5976,0.556776436283003);
#2411=CIRCLE('',#5979,0.93);
#2412=CIRCLE('',#5980,0.93);
#2413=CIRCLE('',#5982,1.3);
#2414=CIRCLE('',#5983,1.3);
#2415=CIRCLE('',#5986,1.24899959967968);
#2416=CIRCLE('',#5988,1.59980467557762);
#2417=CIRCLE('',#5996,0.275);
#2418=CIRCLE('',#5997,0.275);
#2419=CIRCLE('',#5999,0.275);
#2420=CIRCLE('',#6000,0.275);
#2421=CIRCLE('',#6002,0.275);
#2422=CIRCLE('',#6003,0.275);
#2423=CIRCLE('',#6005,0.275);
#2424=CIRCLE('',#6006,0.275);
#2425=CIRCLE('',#6012,1.6);
#2426=CIRCLE('',#6016,1.6);
#2427=CIRCLE('',#6023,1.2);
#2428=CIRCLE('',#6024,0.7);
#2429=CIRCLE('',#6026,1.2);
#2430=CIRCLE('',#6028,0.405);
#2431=CIRCLE('',#6030,0.405);
#2432=CIRCLE('',#6032,0.7);
#2433=CIRCLE('',#6036,0.1);
#2434=CIRCLE('',#6037,0.4);
#2435=CIRCLE('',#6040,0.61);
#2436=CIRCLE('',#6041,0.61);
#2437=CIRCLE('',#6043,0.405);
#2438=CIRCLE('',#6045,0.405);
#2439=CIRCLE('',#6047,1.);
#2440=CIRCLE('',#6048,1.);
#2441=CIRCLE('',#6053,0.3);
#2442=CIRCLE('',#6054,0.3);
#2443=CIRCLE('',#6057,0.3);
#2444=CIRCLE('',#6058,0.3);
#2445=CIRCLE('',#6061,0.225);
#2446=CIRCLE('',#6062,0.225);
#2447=CIRCLE('',#6064,0.225);
#2448=CIRCLE('',#6065,0.225);
#2449=CIRCLE('',#6067,0.225);
#2450=CIRCLE('',#6068,0.225);
#2451=CIRCLE('',#6070,0.225);
#2452=CIRCLE('',#6071,0.225);
#2453=CIRCLE('',#6073,1.01);
#2454=CIRCLE('',#6074,1.01);
#2455=CIRCLE('',#6083,1.11803398874989);
#2456=CIRCLE('',#6084,0.75);
#2457=CIRCLE('',#6086,0.75);
#2458=CIRCLE('',#6088,1.3);
#2459=CIRCLE('',#6089,1.3);
#2460=CIRCLE('',#6102,0.25);
#2461=CIRCLE('',#6103,0.24505);
#2462=CIRCLE('',#6105,0.25);
#2463=CIRCLE('',#6108,0.375);
#2464=CIRCLE('',#6110,0.425);
#2465=CIRCLE('',#6112,0.425);
#2466=CIRCLE('',#6114,0.395);
#2467=CIRCLE('',#6116,0.27);
#2468=CIRCLE('',#6118,0.24505);
#2469=CIRCLE('',#6122,0.285);
#2470=CIRCLE('',#6123,0.265);
#2471=CIRCLE('',#6125,0.265);
#2472=CIRCLE('',#6127,0.5);
#2473=CIRCLE('',#6129,0.5);
#2474=CIRCLE('',#6133,0.38);
#2475=CIRCLE('',#6135,0.38);
#2476=CIRCLE('',#6140,0.2117);
#2477=CIRCLE('',#6141,0.2117);
#2478=CIRCLE('',#6149,0.225);
#2479=CIRCLE('',#6150,0.225);
#2480=CIRCLE('',#6152,0.4);
#2481=CIRCLE('',#6153,0.4);
#2482=CIRCLE('',#6158,0.3);
#2483=CIRCLE('',#6160,0.35);
#2484=CIRCLE('',#6162,0.35);
#2485=CIRCLE('',#6164,0.32);
#2486=CIRCLE('',#6166,0.22);
#2487=CIRCLE('',#6168,0.1954);
#2488=CIRCLE('',#6170,0.1954);
#2489=CIRCLE('',#6172,0.16);
#2490=CIRCLE('',#6184,0.3);
#2491=CIRCLE('',#6185,0.3);
#2492=CIRCLE('',#6225,0.79);
#2493=CIRCLE('',#6226,0.79);
#2494=CIRCLE('',#6228,2.2);
#2495=CIRCLE('',#6229,2.2);
#2496=CIRCLE('',#6234,0.93);
#2497=CIRCLE('',#6235,0.789999999999999);
#2498=CIRCLE('',#6237,0.93);
#2499=CIRCLE('',#6240,0.93);
#2500=CIRCLE('',#6243,0.789999999999999);
#2501=CIRCLE('',#6245,0.93);
#2502=CIRCLE('',#6246,0.93);
#2503=CIRCLE('',#6247,0.93);
#2504=CIRCLE('',#6252,0.79);
#2505=CIRCLE('',#6257,0.79);
#2506=CIRCLE('',#6258,0.93);
#2507=CIRCLE('',#6259,0.93);
#2508=CIRCLE('',#6261,0.93);
#2509=CIRCLE('',#6268,0.789999999999999);
#2510=CIRCLE('',#6270,0.789999999999999);
#2511=CIRCLE('',#6276,1.6);
#2512=CIRCLE('',#6280,1.6);
#2513=CIRCLE('',#6281,1.6);
#2514=CIRCLE('',#6286,0.79);
#2515=CIRCLE('',#6287,0.79);
#2516=CIRCLE('',#6289,1.065);
#2517=CIRCLE('',#6290,1.065);
#2518=CIRCLE('',#6295,0.789999999999999);
#2519=CIRCLE('',#6296,0.789999999999999);
#2520=CIRCLE('',#6298,1.065);
#2521=CIRCLE('',#6299,1.065);
#2522=CIRCLE('',#6304,0.79);
#2523=CIRCLE('',#6305,0.79);
#2524=CIRCLE('',#6307,1.065);
#2525=CIRCLE('',#6308,1.065);
#2526=CIRCLE('',#6314,0.79);
#2527=CIRCLE('',#6315,0.79);
#2528=CIRCLE('',#6316,0.79);
#2529=CIRCLE('',#6318,0.837);
#2530=CIRCLE('',#6319,0.79);
#2531=CIRCLE('',#6320,0.79);
#2532=CIRCLE('',#6322,0.79);
#2533=CIRCLE('',#6324,0.93);
#2534=CIRCLE('',#6326,0.93);
#2535=CIRCLE('',#6328,0.93);
#2536=CIRCLE('',#6329,0.93);
#2537=CIRCLE('',#6332,1.2);
#2538=CIRCLE('',#6333,1.2);
#2539=CIRCLE('',#6334,1.2);
#2540=CIRCLE('',#6335,1.2);
#2541=CIRCLE('',#6338,1.2);
#2542=CIRCLE('',#6340,1.45);
#2543=CIRCLE('',#6342,1.45);
#2544=CIRCLE('',#6345,1.45);
#2545=CIRCLE('',#6346,1.2);
#2546=CIRCLE('',#6348,1.45);
#2547=CIRCLE('',#6353,1.065);
#2548=CIRCLE('',#6355,1.065);
#2549=CIRCLE('',#6363,1.065);
#2550=CIRCLE('',#6365,0.985);
#2551=CIRCLE('',#6366,0.79);
#2552=CIRCLE('',#6369,1.065);
#2553=CIRCLE('',#6371,0.985);
#2554=CIRCLE('',#6373,0.79);
#2555=CIRCLE('',#6377,0.44);
#2556=CIRCLE('',#6378,0.44);
#2557=CIRCLE('',#6380,0.44);
#2558=CIRCLE('',#6381,0.44);
#2559=CIRCLE('',#6383,0.44);
#2560=CIRCLE('',#6384,0.44);
#2561=CIRCLE('',#6386,0.44);
#2562=CIRCLE('',#6387,0.44);
#2563=CIRCLE('',#6389,3.5);
#2564=CIRCLE('',#6390,1.5);
#2565=CIRCLE('',#6392,3.5);
#2566=CIRCLE('',#6394,0.79);
#2567=CIRCLE('',#6395,0.79);
#2568=CIRCLE('',#6397,1.5);
#2569=CIRCLE('',#6402,0.44);
#2570=CIRCLE('',#6403,0.44);
#2571=CIRCLE('',#6405,0.44);
#2572=CIRCLE('',#6406,0.44);
#2573=CIRCLE('',#6408,0.44);
#2574=CIRCLE('',#6409,0.44);
#2575=CIRCLE('',#6411,0.44);
#2576=CIRCLE('',#6412,0.44);
#2577=CIRCLE('',#6414,3.5);
#2578=CIRCLE('',#6415,1.5);
#2579=CIRCLE('',#6417,3.5);
#2580=CIRCLE('',#6419,0.79);
#2581=CIRCLE('',#6420,0.79);
#2582=CIRCLE('',#6422,1.5);
#2583=CIRCLE('',#6427,0.6);
#2584=CIRCLE('',#6429,0.65);
#2585=CIRCLE('',#6431,0.65);
#2586=CIRCLE('',#6433,0.62);
#2587=CIRCLE('',#6435,0.42);
#2588=CIRCLE('',#6437,0.3933);
#2589=CIRCLE('',#6439,0.3933);
#2590=CIRCLE('',#6441,0.32);
#2591=CIRCLE('',#6453,0.42);
#2592=CIRCLE('',#6454,0.42);
#2593=CIRCLE('',#6456,0.8);
#2594=CIRCLE('',#6457,0.8);
#2595=CIRCLE('',#6462,0.6175);
#2596=CIRCLE('',#6464,0.6175);
#2597=CIRCLE('',#6469,0.338975);
#2598=CIRCLE('',#6470,0.338975);
#2599=CIRCLE('',#6511,1.48592563743951);
#2600=CIRCLE('',#6513,1.48592563743951);
#2601=CIRCLE('',#6514,1.48592563743951);
#2602=CIRCLE('',#6516,1.48592563743951);
#2603=CIRCLE('',#6518,1.48592563743951);
#2604=CIRCLE('',#6521,0.75);
#2605=CIRCLE('',#6522,0.75);
#2606=CIRCLE('',#6524,1.5);
#2607=CIRCLE('',#6527,0.165);
#2608=CIRCLE('',#6528,0.165);
#2609=CIRCLE('',#6531,0.4);
#2610=CIRCLE('',#6533,0.4);
#2611=CIRCLE('',#6535,0.4);
#2612=CIRCLE('',#6537,0.4);
#2613=CIRCLE('',#6544,0.4);
#2614=CIRCLE('',#6546,0.4);
#2615=CIRCLE('',#6547,0.4);
#2616=CIRCLE('',#6549,0.4);
#2617=CIRCLE('',#6551,0.4);
#2618=CIRCLE('',#6558,0.4);
#2619=CIRCLE('',#6573,0.225);
#2620=CIRCLE('',#6574,0.225);
#2621=CIRCLE('',#6576,0.6);
#2622=CIRCLE('',#6577,0.6);
#2623=CIRCLE('',#6597,0.1954);
#2624=CIRCLE('',#6599,0.3);
#2625=CIRCLE('',#6601,0.35);
#2626=CIRCLE('',#6603,0.35);
#2627=CIRCLE('',#6605,0.32);
#2628=CIRCLE('',#6607,0.22);
#2629=CIRCLE('',#6609,0.1954);
#2630=VERTEX_POINT('',#8428);
#2631=VERTEX_POINT('',#8430);
#2632=VERTEX_POINT('',#8435);
#2633=VERTEX_POINT('',#8437);
#2634=VERTEX_POINT('',#8442);
#2635=VERTEX_POINT('',#8444);
#2636=VERTEX_POINT('',#8448);
#2637=VERTEX_POINT('',#8450);
#2638=VERTEX_POINT('',#8454);
#2639=VERTEX_POINT('',#8456);
#2640=VERTEX_POINT('',#8460);
#2641=VERTEX_POINT('',#8462);
#2642=VERTEX_POINT('',#8466);
#2643=VERTEX_POINT('',#8467);
#2644=VERTEX_POINT('',#8469);
#2645=VERTEX_POINT('',#8471);
#2646=VERTEX_POINT('',#8475);
#2647=VERTEX_POINT('',#8477);
#2648=VERTEX_POINT('',#8481);
#2649=VERTEX_POINT('',#8483);
#2650=VERTEX_POINT('',#8485);
#2651=VERTEX_POINT('',#8487);
#2652=VERTEX_POINT('',#8491);
#2653=VERTEX_POINT('',#8493);
#2654=VERTEX_POINT('',#8497);
#2655=VERTEX_POINT('',#8499);
#2656=VERTEX_POINT('',#8503);
#2657=VERTEX_POINT('',#8509);
#2658=VERTEX_POINT('',#8511);
#2659=VERTEX_POINT('',#8515);
#2660=VERTEX_POINT('',#8519);
#2661=VERTEX_POINT('',#8527);
#2662=VERTEX_POINT('',#8529);
#2663=VERTEX_POINT('',#8534);
#2664=VERTEX_POINT('',#8536);
#2665=VERTEX_POINT('',#8541);
#2666=VERTEX_POINT('',#8543);
#2667=VERTEX_POINT('',#8547);
#2668=VERTEX_POINT('',#8549);
#2669=VERTEX_POINT('',#8553);
#2670=VERTEX_POINT('',#8555);
#2671=VERTEX_POINT('',#8559);
#2672=VERTEX_POINT('',#8561);
#2673=VERTEX_POINT('',#8565);
#2674=VERTEX_POINT('',#8566);
#2675=VERTEX_POINT('',#8568);
#2676=VERTEX_POINT('',#8570);
#2677=VERTEX_POINT('',#8574);
#2678=VERTEX_POINT('',#8576);
#2679=VERTEX_POINT('',#8580);
#2680=VERTEX_POINT('',#8582);
#2681=VERTEX_POINT('',#8584);
#2682=VERTEX_POINT('',#8586);
#2683=VERTEX_POINT('',#8590);
#2684=VERTEX_POINT('',#8592);
#2685=VERTEX_POINT('',#8596);
#2686=VERTEX_POINT('',#8598);
#2687=VERTEX_POINT('',#8603);
#2688=VERTEX_POINT('',#8608);
#2689=VERTEX_POINT('',#8609);
#2690=VERTEX_POINT('',#8614);
#2691=VERTEX_POINT('',#8618);
#2692=VERTEX_POINT('',#8626);
#2693=VERTEX_POINT('',#8628);
#2694=VERTEX_POINT('',#8632);
#2695=VERTEX_POINT('',#8634);
#2696=VERTEX_POINT('',#8638);
#2697=VERTEX_POINT('',#8640);
#2698=VERTEX_POINT('',#8644);
#2699=VERTEX_POINT('',#8646);
#2700=VERTEX_POINT('',#8650);
#2701=VERTEX_POINT('',#8651);
#2702=VERTEX_POINT('',#8653);
#2703=VERTEX_POINT('',#8655);
#2704=VERTEX_POINT('',#8659);
#2705=VERTEX_POINT('',#8660);
#2706=VERTEX_POINT('',#8662);
#2707=VERTEX_POINT('',#8664);
#2708=VERTEX_POINT('',#8668);
#2709=VERTEX_POINT('',#8670);
#2710=VERTEX_POINT('',#8674);
#2711=VERTEX_POINT('',#8676);
#2712=VERTEX_POINT('',#8681);
#2713=VERTEX_POINT('',#8683);
#2714=VERTEX_POINT('',#8685);
#2715=VERTEX_POINT('',#8687);
#2716=VERTEX_POINT('',#8691);
#2717=VERTEX_POINT('',#8695);
#2718=VERTEX_POINT('',#8701);
#2719=VERTEX_POINT('',#8705);
#2720=VERTEX_POINT('',#8713);
#2721=VERTEX_POINT('',#8715);
#2722=VERTEX_POINT('',#8718);
#2723=VERTEX_POINT('',#8722);
#2724=VERTEX_POINT('',#8725);
#2725=VERTEX_POINT('',#8729);
#2726=VERTEX_POINT('',#8735);
#2727=VERTEX_POINT('',#8740);
#2728=VERTEX_POINT('',#8742);
#2729=VERTEX_POINT('',#8746);
#2730=VERTEX_POINT('',#8749);
#2731=VERTEX_POINT('',#8753);
#2732=VERTEX_POINT('',#8755);
#2733=VERTEX_POINT('',#8762);
#2734=VERTEX_POINT('',#8764);
#2735=VERTEX_POINT('',#8769);
#2736=VERTEX_POINT('',#8771);
#2737=VERTEX_POINT('',#8776);
#2738=VERTEX_POINT('',#8778);
#2739=VERTEX_POINT('',#8782);
#2740=VERTEX_POINT('',#8784);
#2741=VERTEX_POINT('',#8788);
#2742=VERTEX_POINT('',#8790);
#2743=VERTEX_POINT('',#8794);
#2744=VERTEX_POINT('',#8796);
#2745=VERTEX_POINT('',#8800);
#2746=VERTEX_POINT('',#8802);
#2747=VERTEX_POINT('',#8806);
#2748=VERTEX_POINT('',#8807);
#2749=VERTEX_POINT('',#8809);
#2750=VERTEX_POINT('',#8811);
#2751=VERTEX_POINT('',#8815);
#2752=VERTEX_POINT('',#8817);
#2753=VERTEX_POINT('',#8821);
#2754=VERTEX_POINT('',#8823);
#2755=VERTEX_POINT('',#8833);
#2756=VERTEX_POINT('',#8835);
#2757=VERTEX_POINT('',#8838);
#2758=VERTEX_POINT('',#8842);
#2759=VERTEX_POINT('',#8844);
#2760=VERTEX_POINT('',#8851);
#2761=VERTEX_POINT('',#8852);
#2762=VERTEX_POINT('',#8854);
#2763=VERTEX_POINT('',#8856);
#2764=VERTEX_POINT('',#8860);
#2765=VERTEX_POINT('',#8862);
#2766=VERTEX_POINT('',#8866);
#2767=VERTEX_POINT('',#8868);
#2768=VERTEX_POINT('',#8872);
#2769=VERTEX_POINT('',#8874);
#2770=VERTEX_POINT('',#8878);
#2771=VERTEX_POINT('',#8880);
#2772=VERTEX_POINT('',#8889);
#2773=VERTEX_POINT('',#8891);
#2774=VERTEX_POINT('',#8894);
#2775=VERTEX_POINT('',#8899);
#2776=VERTEX_POINT('',#8902);
#2777=VERTEX_POINT('',#8906);
#2778=VERTEX_POINT('',#8910);
#2779=VERTEX_POINT('',#8914);
#2780=VERTEX_POINT('',#8917);
#2781=VERTEX_POINT('',#8924);
#2782=VERTEX_POINT('',#8926);
#2783=VERTEX_POINT('',#8930);
#2784=VERTEX_POINT('',#8934);
#2785=VERTEX_POINT('',#8937);
#2786=VERTEX_POINT('',#8943);
#2787=VERTEX_POINT('',#8944);
#2788=VERTEX_POINT('',#8948);
#2789=VERTEX_POINT('',#8952);
#2790=VERTEX_POINT('',#8955);
#2791=VERTEX_POINT('',#8959);
#2792=VERTEX_POINT('',#8963);
#2793=VERTEX_POINT('',#8971);
#2794=VERTEX_POINT('',#8973);
#2795=VERTEX_POINT('',#8975);
#2796=VERTEX_POINT('',#8979);
#2797=VERTEX_POINT('',#8983);
#2798=VERTEX_POINT('',#8987);
#2799=VERTEX_POINT('',#8991);
#2800=VERTEX_POINT('',#9006);
#2801=VERTEX_POINT('',#9008);
#2802=VERTEX_POINT('',#9020);
#2803=VERTEX_POINT('',#9022);
#2804=VERTEX_POINT('',#9026);
#2805=VERTEX_POINT('',#9028);
#2806=VERTEX_POINT('',#9035);
#2807=VERTEX_POINT('',#9038);
#2808=VERTEX_POINT('',#9042);
#2809=VERTEX_POINT('',#9046);
#2810=VERTEX_POINT('',#9050);
#2811=VERTEX_POINT('',#9053);
#2812=VERTEX_POINT('',#9057);
#2813=VERTEX_POINT('',#9061);
#2814=VERTEX_POINT('',#9066);
#2815=VERTEX_POINT('',#9067);
#2816=VERTEX_POINT('',#9069);
#2817=VERTEX_POINT('',#9071);
#2818=VERTEX_POINT('',#9075);
#2819=VERTEX_POINT('',#9077);
#2820=VERTEX_POINT('',#9081);
#2821=VERTEX_POINT('',#9083);
#2822=VERTEX_POINT('',#9087);
#2823=VERTEX_POINT('',#9089);
#2824=VERTEX_POINT('',#9093);
#2825=VERTEX_POINT('',#9095);
#2826=VERTEX_POINT('',#9105);
#2827=VERTEX_POINT('',#9107);
#2828=VERTEX_POINT('',#9149);
#2829=VERTEX_POINT('',#9151);
#2830=VERTEX_POINT('',#9155);
#2831=VERTEX_POINT('',#9157);
#2832=VERTEX_POINT('',#9164);
#2833=VERTEX_POINT('',#9165);
#2834=VERTEX_POINT('',#9167);
#2835=VERTEX_POINT('',#9169);
#2836=VERTEX_POINT('',#9173);
#2837=VERTEX_POINT('',#9175);
#2838=VERTEX_POINT('',#9178);
#2839=VERTEX_POINT('',#9180);
#2840=VERTEX_POINT('',#9184);
#2841=VERTEX_POINT('',#9186);
#2842=VERTEX_POINT('',#9190);
#2843=VERTEX_POINT('',#9192);
#2844=VERTEX_POINT('',#9197);
#2845=VERTEX_POINT('',#9203);
#2846=VERTEX_POINT('',#9208);
#2847=VERTEX_POINT('',#9212);
#2848=VERTEX_POINT('',#9216);
#2849=VERTEX_POINT('',#9218);
#2850=VERTEX_POINT('',#9221);
#2851=VERTEX_POINT('',#9223);
#2852=VERTEX_POINT('',#9233);
#2853=VERTEX_POINT('',#9234);
#2854=VERTEX_POINT('',#9236);
#2855=VERTEX_POINT('',#9238);
#2856=VERTEX_POINT('',#9244);
#2857=VERTEX_POINT('',#9247);
#2858=VERTEX_POINT('',#9254);
#2859=VERTEX_POINT('',#9256);
#2860=VERTEX_POINT('',#9260);
#2861=VERTEX_POINT('',#9262);
#2862=VERTEX_POINT('',#9269);
#2863=VERTEX_POINT('',#9271);
#2864=VERTEX_POINT('',#9275);
#2865=VERTEX_POINT('',#9277);
#2866=VERTEX_POINT('',#9284);
#2867=VERTEX_POINT('',#9286);
#2868=VERTEX_POINT('',#9290);
#2869=VERTEX_POINT('',#9292);
#2870=VERTEX_POINT('',#9299);
#2871=VERTEX_POINT('',#9300);
#2872=VERTEX_POINT('',#9302);
#2873=VERTEX_POINT('',#9304);
#2874=VERTEX_POINT('',#9309);
#2875=VERTEX_POINT('',#9310);
#2876=VERTEX_POINT('',#9312);
#2877=VERTEX_POINT('',#9316);
#2878=VERTEX_POINT('',#9320);
#2879=VERTEX_POINT('',#9323);
#2880=VERTEX_POINT('',#9327);
#2881=VERTEX_POINT('',#9329);
#2882=VERTEX_POINT('',#9334);
#2883=VERTEX_POINT('',#9335);
#2884=VERTEX_POINT('',#9337);
#2885=VERTEX_POINT('',#9339);
#2886=VERTEX_POINT('',#9344);
#2887=VERTEX_POINT('',#9348);
#2888=VERTEX_POINT('',#9351);
#2889=VERTEX_POINT('',#9356);
#2890=VERTEX_POINT('',#9358);
#2891=VERTEX_POINT('',#9361);
#2892=VERTEX_POINT('',#9369);
#2893=VERTEX_POINT('',#9370);
#2894=VERTEX_POINT('',#9372);
#2895=VERTEX_POINT('',#9374);
#2896=VERTEX_POINT('',#9376);
#2897=VERTEX_POINT('',#9378);
#2898=VERTEX_POINT('',#9381);
#2899=VERTEX_POINT('',#9384);
#2900=VERTEX_POINT('',#9385);
#2901=VERTEX_POINT('',#9387);
#2902=VERTEX_POINT('',#9389);
#2903=VERTEX_POINT('',#9391);
#2904=VERTEX_POINT('',#9393);
#2905=VERTEX_POINT('',#9396);
#2906=VERTEX_POINT('',#9411);
#2907=VERTEX_POINT('',#9415);
#2908=VERTEX_POINT('',#9417);
#2909=VERTEX_POINT('',#9422);
#2910=VERTEX_POINT('',#9426);
#2911=VERTEX_POINT('',#9430);
#2912=VERTEX_POINT('',#9436);
#2913=VERTEX_POINT('',#9438);
#2914=VERTEX_POINT('',#9442);
#2915=VERTEX_POINT('',#9444);
#2916=VERTEX_POINT('',#9448);
#2917=VERTEX_POINT('',#9450);
#2918=VERTEX_POINT('',#9454);
#2919=VERTEX_POINT('',#9456);
#2920=VERTEX_POINT('',#9460);
#2921=VERTEX_POINT('',#9462);
#2922=VERTEX_POINT('',#9465);
#2923=VERTEX_POINT('',#9469);
#2924=VERTEX_POINT('',#9471);
#2925=VERTEX_POINT('',#9475);
#2926=VERTEX_POINT('',#9482);
#2927=VERTEX_POINT('',#9484);
#2928=VERTEX_POINT('',#9488);
#2929=VERTEX_POINT('',#9490);
#2930=VERTEX_POINT('',#9494);
#2931=VERTEX_POINT('',#9496);
#2932=VERTEX_POINT('',#9500);
#2933=VERTEX_POINT('',#9502);
#2934=VERTEX_POINT('',#9506);
#2935=VERTEX_POINT('',#9508);
#2936=VERTEX_POINT('',#9511);
#2937=VERTEX_POINT('',#9515);
#2938=VERTEX_POINT('',#9517);
#2939=VERTEX_POINT('',#9521);
#2940=VERTEX_POINT('',#9528);
#2941=VERTEX_POINT('',#9531);
#2942=VERTEX_POINT('',#9535);
#2943=VERTEX_POINT('',#9539);
#2944=VERTEX_POINT('',#9543);
#2945=VERTEX_POINT('',#9546);
#2946=VERTEX_POINT('',#9550);
#2947=VERTEX_POINT('',#9554);
#2948=VERTEX_POINT('',#9559);
#2949=VERTEX_POINT('',#9560);
#2950=VERTEX_POINT('',#9562);
#2951=VERTEX_POINT('',#9564);
#2952=VERTEX_POINT('',#9568);
#2953=VERTEX_POINT('',#9570);
#2954=VERTEX_POINT('',#9574);
#2955=VERTEX_POINT('',#9576);
#2956=VERTEX_POINT('',#9580);
#2957=VERTEX_POINT('',#9582);
#2958=VERTEX_POINT('',#9586);
#2959=VERTEX_POINT('',#9588);
#2960=VERTEX_POINT('',#9598);
#2961=VERTEX_POINT('',#9600);
#2962=VERTEX_POINT('',#9604);
#2963=VERTEX_POINT('',#9606);
#2964=VERTEX_POINT('',#9613);
#2965=VERTEX_POINT('',#9614);
#2966=VERTEX_POINT('',#9618);
#2967=VERTEX_POINT('',#9622);
#2968=VERTEX_POINT('',#9625);
#2969=VERTEX_POINT('',#9629);
#2970=VERTEX_POINT('',#9633);
#2971=VERTEX_POINT('',#9641);
#2972=VERTEX_POINT('',#9643);
#2973=VERTEX_POINT('',#9645);
#2974=VERTEX_POINT('',#9649);
#2975=VERTEX_POINT('',#9653);
#2976=VERTEX_POINT('',#9657);
#2977=VERTEX_POINT('',#9661);
#2978=VERTEX_POINT('',#9676);
#2979=VERTEX_POINT('',#9678);
#2980=VERTEX_POINT('',#9723);
#2981=VERTEX_POINT('',#9724);
#2982=VERTEX_POINT('',#9726);
#2983=VERTEX_POINT('',#9728);
#2984=VERTEX_POINT('',#9732);
#2985=VERTEX_POINT('',#9734);
#2986=VERTEX_POINT('',#9736);
#2987=VERTEX_POINT('',#9740);
#2988=VERTEX_POINT('',#9742);
#2989=VERTEX_POINT('',#9750);
#2990=VERTEX_POINT('',#9752);
#2991=VERTEX_POINT('',#9756);
#2992=VERTEX_POINT('',#9760);
#2993=VERTEX_POINT('',#9762);
#2994=VERTEX_POINT('',#9767);
#2995=VERTEX_POINT('',#9768);
#2996=VERTEX_POINT('',#9770);
#2997=VERTEX_POINT('',#9774);
#2998=VERTEX_POINT('',#9775);
#2999=VERTEX_POINT('',#9777);
#3000=VERTEX_POINT('',#9781);
#3001=VERTEX_POINT('',#9782);
#3002=VERTEX_POINT('',#9784);
#3003=VERTEX_POINT('',#9788);
#3004=VERTEX_POINT('',#9789);
#3005=VERTEX_POINT('',#9791);
#3006=VERTEX_POINT('',#9796);
#3007=VERTEX_POINT('',#9798);
#3008=VERTEX_POINT('',#9803);
#3009=VERTEX_POINT('',#9808);
#3010=VERTEX_POINT('',#9818);
#3011=VERTEX_POINT('',#9826);
#3012=VERTEX_POINT('',#9827);
#3013=VERTEX_POINT('',#9829);
#3014=VERTEX_POINT('',#9831);
#3015=VERTEX_POINT('',#9835);
#3016=VERTEX_POINT('',#9837);
#3017=VERTEX_POINT('',#9841);
#3018=VERTEX_POINT('',#9843);
#3019=VERTEX_POINT('',#9851);
#3020=VERTEX_POINT('',#9857);
#3021=VERTEX_POINT('',#9858);
#3022=VERTEX_POINT('',#9860);
#3023=VERTEX_POINT('',#9862);
#3024=VERTEX_POINT('',#9866);
#3025=VERTEX_POINT('',#9868);
#3026=VERTEX_POINT('',#9872);
#3027=VERTEX_POINT('',#9874);
#3028=VERTEX_POINT('',#9881);
#3029=VERTEX_POINT('',#9882);
#3030=VERTEX_POINT('',#9884);
#3031=VERTEX_POINT('',#9886);
#3032=VERTEX_POINT('',#9890);
#3033=VERTEX_POINT('',#9892);
#3034=VERTEX_POINT('',#9896);
#3035=VERTEX_POINT('',#9898);
#3036=VERTEX_POINT('',#9908);
#3037=VERTEX_POINT('',#9910);
#3038=VERTEX_POINT('',#9914);
#3039=VERTEX_POINT('',#9916);
#3040=VERTEX_POINT('',#9923);
#3041=VERTEX_POINT('',#9924);
#3042=VERTEX_POINT('',#9926);
#3043=VERTEX_POINT('',#9928);
#3044=VERTEX_POINT('',#9932);
#3045=VERTEX_POINT('',#9934);
#3046=VERTEX_POINT('',#9938);
#3047=VERTEX_POINT('',#9940);
#3048=VERTEX_POINT('',#9950);
#3049=VERTEX_POINT('',#9951);
#3050=VERTEX_POINT('',#9953);
#3051=VERTEX_POINT('',#9955);
#3052=VERTEX_POINT('',#9959);
#3053=VERTEX_POINT('',#9961);
#3054=VERTEX_POINT('',#9965);
#3055=VERTEX_POINT('',#9967);
#3056=VERTEX_POINT('',#9971);
#3057=VERTEX_POINT('',#9973);
#3058=VERTEX_POINT('',#9977);
#3059=VERTEX_POINT('',#9979);
#3060=VERTEX_POINT('',#9988);
#3061=VERTEX_POINT('',#9991);
#3062=VERTEX_POINT('',#9994);
#3063=VERTEX_POINT('',#9998);
#3064=VERTEX_POINT('',#10002);
#3065=VERTEX_POINT('',#10006);
#3066=VERTEX_POINT('',#10009);
#3067=EDGE_CURVE('',#2630,#2630,#2375,.T.);
#3068=EDGE_CURVE('',#2630,#2631,#1623,.T.);
#3069=EDGE_CURVE('',#2631,#2631,#2376,.T.);
#3070=EDGE_CURVE('',#2632,#2632,#2377,.T.);
#3071=EDGE_CURVE('',#2632,#2633,#1624,.T.);
#3072=EDGE_CURVE('',#2633,#2633,#2378,.T.);
#3073=EDGE_CURVE('',#2634,#2634,#2379,.T.);
#3074=EDGE_CURVE('',#2634,#2635,#1625,.T.);
#3075=EDGE_CURVE('',#2635,#2635,#2380,.T.);
#3076=EDGE_CURVE('',#2636,#2636,#2381,.T.);
#3077=EDGE_CURVE('',#2636,#2637,#1626,.T.);
#3078=EDGE_CURVE('',#2637,#2637,#2382,.T.);
#3079=EDGE_CURVE('',#2638,#2638,#2383,.T.);
#3080=EDGE_CURVE('',#2638,#2639,#1627,.T.);
#3081=EDGE_CURVE('',#2639,#2639,#2384,.T.);
#3082=EDGE_CURVE('',#2640,#2640,#2385,.T.);
#3083=EDGE_CURVE('',#2640,#2641,#1628,.T.);
#3084=EDGE_CURVE('',#2641,#2641,#2386,.T.);
#3085=EDGE_CURVE('',#2642,#2643,#1629,.T.);
#3086=EDGE_CURVE('',#2644,#2642,#2387,.T.);
#3087=EDGE_CURVE('',#2645,#2644,#1630,.T.);
#3088=EDGE_CURVE('',#2643,#2645,#2388,.T.);
#3089=EDGE_CURVE('',#2646,#2642,#1631,.T.);
#3090=EDGE_CURVE('',#2647,#2646,#2389,.T.);
#3091=EDGE_CURVE('',#2644,#2647,#1632,.T.);
#3092=EDGE_CURVE('',#2645,#2648,#1633,.T.);
#3093=EDGE_CURVE('',#2648,#2649,#1634,.T.);
#3094=EDGE_CURVE('',#2649,#2650,#1635,.T.);
#3095=EDGE_CURVE('',#2650,#2651,#1636,.T.);
#3096=EDGE_CURVE('',#2651,#2643,#1637,.T.);
#3097=EDGE_CURVE('',#2652,#2652,#2390,.T.);
#3098=EDGE_CURVE('',#2652,#2653,#1638,.T.);
#3099=EDGE_CURVE('',#2653,#2653,#2391,.T.);
#3100=EDGE_CURVE('',#2654,#2654,#2392,.T.);
#3101=EDGE_CURVE('',#2654,#2655,#1639,.T.);
#3102=EDGE_CURVE('',#2655,#2655,#2393,.T.);
#3103=EDGE_CURVE('',#2656,#2656,#2394,.T.);
#3104=EDGE_CURVE('',#2647,#2646,#2395,.T.);
#3105=EDGE_CURVE('',#2657,#2651,#1640,.T.);
#3106=EDGE_CURVE('',#2657,#2658,#1641,.T.);
#3107=EDGE_CURVE('',#2658,#2648,#1642,.T.);
#3108=EDGE_CURVE('',#2659,#2657,#1643,.T.);
#3109=EDGE_CURVE('',#2659,#2650,#1644,.T.);
#3110=EDGE_CURVE('',#2660,#2659,#1645,.T.);
#3111=EDGE_CURVE('',#2660,#2649,#1646,.T.);
#3112=EDGE_CURVE('',#2658,#2660,#1647,.T.);
#3113=EDGE_CURVE('',#2661,#2661,#2396,.T.);
#3114=EDGE_CURVE('',#2661,#2662,#1648,.T.);
#3115=EDGE_CURVE('',#2662,#2662,#2397,.T.);
#3116=EDGE_CURVE('',#2663,#2663,#2398,.T.);
#3117=EDGE_CURVE('',#2663,#2664,#1649,.T.);
#3118=EDGE_CURVE('',#2664,#2664,#2399,.T.);
#3119=EDGE_CURVE('',#2665,#2665,#2400,.T.);
#3120=EDGE_CURVE('',#2665,#2666,#1650,.T.);
#3121=EDGE_CURVE('',#2666,#2666,#2401,.T.);
#3122=EDGE_CURVE('',#2667,#2667,#2402,.T.);
#3123=EDGE_CURVE('',#2667,#2668,#1651,.T.);
#3124=EDGE_CURVE('',#2668,#2668,#2403,.T.);
#3125=EDGE_CURVE('',#2669,#2669,#2404,.T.);
#3126=EDGE_CURVE('',#2669,#2670,#1652,.T.);
#3127=EDGE_CURVE('',#2670,#2670,#2405,.T.);
#3128=EDGE_CURVE('',#2671,#2671,#2406,.T.);
#3129=EDGE_CURVE('',#2671,#2672,#1653,.T.);
#3130=EDGE_CURVE('',#2672,#2672,#2407,.T.);
#3131=EDGE_CURVE('',#2673,#2674,#1654,.T.);
#3132=EDGE_CURVE('',#2675,#2673,#2408,.T.);
#3133=EDGE_CURVE('',#2676,#2675,#1655,.T.);
#3134=EDGE_CURVE('',#2674,#2676,#2409,.T.);
#3135=EDGE_CURVE('',#2677,#2673,#1656,.T.);
#3136=EDGE_CURVE('',#2678,#2677,#2410,.T.);
#3137=EDGE_CURVE('',#2675,#2678,#1657,.T.);
#3138=EDGE_CURVE('',#2676,#2679,#1658,.T.);
#3139=EDGE_CURVE('',#2679,#2680,#1659,.T.);
#3140=EDGE_CURVE('',#2680,#2681,#1660,.T.);
#3141=EDGE_CURVE('',#2681,#2682,#1661,.T.);
#3142=EDGE_CURVE('',#2682,#2674,#1662,.T.);
#3143=EDGE_CURVE('',#2683,#2683,#2411,.T.);
#3144=EDGE_CURVE('',#2683,#2684,#1663,.T.);
#3145=EDGE_CURVE('',#2684,#2684,#2412,.T.);
#3146=EDGE_CURVE('',#2685,#2685,#2413,.T.);
#3147=EDGE_CURVE('',#2685,#2686,#1664,.T.);
#3148=EDGE_CURVE('',#2686,#2686,#2414,.T.);
#3149=EDGE_CURVE('',#2687,#2687,#2415,.T.);
#3150=EDGE_CURVE('',#2678,#2677,#2416,.T.);
#3151=EDGE_CURVE('',#2688,#2689,#1665,.T.);
#3152=EDGE_CURVE('',#2689,#2681,#1666,.T.);
#3153=EDGE_CURVE('',#2688,#2680,#1667,.T.);
#3154=EDGE_CURVE('',#2690,#2688,#1668,.T.);
#3155=EDGE_CURVE('',#2690,#2679,#1669,.T.);
#3156=EDGE_CURVE('',#2691,#2682,#1670,.T.);
#3157=EDGE_CURVE('',#2691,#2690,#1671,.T.);
#3158=EDGE_CURVE('',#2689,#2691,#1672,.T.);
#3159=EDGE_CURVE('',#2692,#2692,#2417,.T.);
#3160=EDGE_CURVE('',#2692,#2693,#1673,.T.);
#3161=EDGE_CURVE('',#2693,#2693,#2418,.T.);
#3162=EDGE_CURVE('',#2694,#2694,#2419,.T.);
#3163=EDGE_CURVE('',#2694,#2695,#1674,.T.);
#3164=EDGE_CURVE('',#2695,#2695,#2420,.T.);
#3165=EDGE_CURVE('',#2696,#2696,#2421,.T.);
#3166=EDGE_CURVE('',#2696,#2697,#1675,.T.);
#3167=EDGE_CURVE('',#2697,#2697,#2422,.T.);
#3168=EDGE_CURVE('',#2698,#2698,#2423,.T.);
#3169=EDGE_CURVE('',#2698,#2699,#1676,.T.);
#3170=EDGE_CURVE('',#2699,#2699,#2424,.T.);
#3171=EDGE_CURVE('',#2700,#2701,#1677,.T.);
#3172=EDGE_CURVE('',#2700,#2702,#1678,.T.);
#3173=EDGE_CURVE('',#2703,#2702,#1679,.T.);
#3174=EDGE_CURVE('',#2701,#2703,#1680,.T.);
#3175=EDGE_CURVE('',#2704,#2705,#1681,.T.);
#3176=EDGE_CURVE('',#2704,#2706,#1682,.T.);
#3177=EDGE_CURVE('',#2707,#2706,#1683,.T.);
#3178=EDGE_CURVE('',#2705,#2707,#1684,.T.);
#3179=EDGE_CURVE('',#2708,#2700,#1685,.T.);
#3180=EDGE_CURVE('',#2709,#2708,#1686,.T.);
#3181=EDGE_CURVE('',#2702,#2709,#1687,.T.);
#3182=EDGE_CURVE('',#2710,#2704,#1688,.T.);
#3183=EDGE_CURVE('',#2711,#2710,#1689,.T.);
#3184=EDGE_CURVE('',#2706,#2711,#1690,.T.);
#3185=EDGE_CURVE('',#2709,#2707,#2425,.T.);
#3186=EDGE_CURVE('',#2711,#2712,#1691,.T.);
#3187=EDGE_CURVE('',#2712,#2713,#1692,.T.);
#3188=EDGE_CURVE('',#2713,#2714,#1693,.T.);
#3189=EDGE_CURVE('',#2714,#2715,#1694,.T.);
#3190=EDGE_CURVE('',#2715,#2703,#1695,.T.);
#3191=EDGE_CURVE('',#2716,#2710,#1696,.T.);
#3192=EDGE_CURVE('',#2716,#2712,#1697,.T.);
#3193=EDGE_CURVE('',#2717,#2715,#1698,.T.);
#3194=EDGE_CURVE('',#2701,#2717,#1699,.T.);
#3195=EDGE_CURVE('',#2705,#2708,#2426,.T.);
#3196=EDGE_CURVE('',#2717,#2718,#1700,.T.);
#3197=EDGE_CURVE('',#2718,#2714,#1701,.T.);
#3198=EDGE_CURVE('',#2718,#2719,#1702,.T.);
#3199=EDGE_CURVE('',#2719,#2713,#1703,.T.);
#3200=EDGE_CURVE('',#2719,#2716,#1704,.T.);
#3201=EDGE_CURVE('',#2720,#2720,#2427,.T.);
#3202=EDGE_CURVE('',#2721,#2721,#2428,.T.);
#3203=EDGE_CURVE('',#2722,#2722,#2429,.T.);
#3204=EDGE_CURVE('',#2722,#2720,#1705,.T.);
#3205=EDGE_CURVE('',#2723,#2723,#2430,.T.);
#3206=EDGE_CURVE('',#2723,#2724,#1706,.T.);
#3207=EDGE_CURVE('',#2724,#2724,#2431,.T.);
#3208=EDGE_CURVE('',#2721,#2725,#1707,.T.);
#3209=EDGE_CURVE('',#2725,#2725,#2432,.T.);
#3210=EDGE_CURVE('',#2726,#2726,#2433,.T.);
#3211=EDGE_CURVE('',#2726,#2726,#2434,.T.);
#3212=EDGE_CURVE('',#2727,#2727,#2435,.T.);
#3213=EDGE_CURVE('',#2727,#2728,#1708,.T.);
#3214=EDGE_CURVE('',#2728,#2728,#2436,.T.);
#3215=EDGE_CURVE('',#2729,#2729,#2437,.T.);
#3216=EDGE_CURVE('',#2730,#2730,#2438,.T.);
#3217=EDGE_CURVE('',#2730,#2729,#1709,.T.);
#3218=EDGE_CURVE('',#2731,#2731,#2439,.T.);
#3219=EDGE_CURVE('',#2731,#2732,#1710,.T.);
#3220=EDGE_CURVE('',#2732,#2732,#2440,.T.);
#3221=EDGE_CURVE('',#2733,#2733,#2441,.T.);
#3222=EDGE_CURVE('',#2733,#2734,#1711,.T.);
#3223=EDGE_CURVE('',#2734,#2734,#2442,.T.);
#3224=EDGE_CURVE('',#2735,#2735,#2443,.T.);
#3225=EDGE_CURVE('',#2735,#2736,#1712,.T.);
#3226=EDGE_CURVE('',#2736,#2736,#2444,.T.);
#3227=EDGE_CURVE('',#2737,#2737,#2445,.T.);
#3228=EDGE_CURVE('',#2737,#2738,#1713,.T.);
#3229=EDGE_CURVE('',#2738,#2738,#2446,.T.);
#3230=EDGE_CURVE('',#2739,#2739,#2447,.T.);
#3231=EDGE_CURVE('',#2739,#2740,#1714,.T.);
#3232=EDGE_CURVE('',#2740,#2740,#2448,.T.);
#3233=EDGE_CURVE('',#2741,#2741,#2449,.T.);
#3234=EDGE_CURVE('',#2741,#2742,#1715,.T.);
#3235=EDGE_CURVE('',#2742,#2742,#2450,.T.);
#3236=EDGE_CURVE('',#2743,#2743,#2451,.T.);
#3237=EDGE_CURVE('',#2743,#2744,#1716,.T.);
#3238=EDGE_CURVE('',#2744,#2744,#2452,.T.);
#3239=EDGE_CURVE('',#2745,#2745,#2453,.T.);
#3240=EDGE_CURVE('',#2745,#2746,#1717,.T.);
#3241=EDGE_CURVE('',#2746,#2746,#2454,.T.);
#3242=EDGE_CURVE('',#2747,#2748,#1718,.T.);
#3243=EDGE_CURVE('',#2748,#2749,#1719,.T.);
#3244=EDGE_CURVE('',#2750,#2749,#1720,.T.);
#3245=EDGE_CURVE('',#2747,#2750,#1721,.T.);
#3246=EDGE_CURVE('',#2751,#2747,#1722,.T.);
#3247=EDGE_CURVE('',#2752,#2750,#1723,.T.);
#3248=EDGE_CURVE('',#2751,#2752,#1724,.T.);
#3249=EDGE_CURVE('',#2753,#2751,#1725,.T.);
#3250=EDGE_CURVE('',#2754,#2752,#1726,.T.);
#3251=EDGE_CURVE('',#2753,#2754,#1727,.T.);
#3252=EDGE_CURVE('',#2748,#2753,#1728,.T.);
#3253=EDGE_CURVE('',#2749,#2754,#1729,.T.);
#3254=EDGE_CURVE('',#2755,#2755,#2455,.T.);
#3255=EDGE_CURVE('',#2756,#2756,#2456,.T.);
#3256=EDGE_CURVE('',#2756,#2757,#1730,.T.);
#3257=EDGE_CURVE('',#2757,#2757,#2457,.T.);
#3258=EDGE_CURVE('',#2758,#2758,#2458,.T.);
#3259=EDGE_CURVE('',#2758,#2759,#1731,.T.);
#3260=EDGE_CURVE('',#2759,#2759,#2459,.T.);
#3261=EDGE_CURVE('',#2760,#2761,#1732,.T.);
#3262=EDGE_CURVE('',#2761,#2762,#1733,.T.);
#3263=EDGE_CURVE('',#2762,#2763,#1734,.T.);
#3264=EDGE_CURVE('',#2760,#2763,#1735,.T.);
#3265=EDGE_CURVE('',#2761,#2764,#1736,.T.);
#3266=EDGE_CURVE('',#2764,#2765,#1737,.T.);
#3267=EDGE_CURVE('',#2765,#2762,#1738,.T.);
#3268=EDGE_CURVE('',#2764,#2766,#1739,.T.);
#3269=EDGE_CURVE('',#2766,#2767,#1740,.T.);
#3270=EDGE_CURVE('',#2767,#2765,#1741,.T.);
#3271=EDGE_CURVE('',#2766,#2768,#1742,.T.);
#3272=EDGE_CURVE('',#2768,#2769,#1743,.T.);
#3273=EDGE_CURVE('',#2769,#2767,#1744,.T.);
#3274=EDGE_CURVE('',#2768,#2770,#1745,.T.);
#3275=EDGE_CURVE('',#2770,#2771,#1746,.T.);
#3276=EDGE_CURVE('',#2771,#2769,#1747,.T.);
#3277=EDGE_CURVE('',#2770,#2760,#1748,.T.);
#3278=EDGE_CURVE('',#2763,#2771,#1749,.T.);
#3279=EDGE_CURVE('',#2772,#2772,#2460,.T.);
#3280=EDGE_CURVE('',#2773,#2773,#2461,.T.);
#3281=EDGE_CURVE('',#2772,#2774,#1750,.T.);
#3282=EDGE_CURVE('',#2774,#2774,#2462,.T.);
#3283=EDGE_CURVE('',#2775,#2775,#2463,.T.);
#3284=EDGE_CURVE('',#2776,#2776,#2464,.T.);
#3285=EDGE_CURVE('',#2776,#2775,#1751,.T.);
#3286=EDGE_CURVE('',#2777,#2777,#2465,.T.);
#3287=EDGE_CURVE('',#2777,#2776,#1752,.T.);
#3288=EDGE_CURVE('',#2778,#2778,#2466,.T.);
#3289=EDGE_CURVE('',#2778,#2777,#1753,.T.);
#3290=EDGE_CURVE('',#2779,#2779,#2467,.T.);
#3291=EDGE_CURVE('',#2780,#2780,#2468,.F.);
#3292=EDGE_CURVE('',#2780,#2779,#1754,.T.);
#3293=EDGE_CURVE('',#2773,#2780,#1755,.T.);
#3294=EDGE_CURVE('',#2781,#2781,#2469,.T.);
#3295=EDGE_CURVE('',#2781,#2782,#1756,.T.);
#3296=EDGE_CURVE('',#2782,#2782,#2470,.T.);
#3297=EDGE_CURVE('',#2782,#2783,#1757,.T.);
#3298=EDGE_CURVE('',#2783,#2783,#2471,.T.);
#3299=EDGE_CURVE('',#2784,#2784,#2472,.T.);
#3300=EDGE_CURVE('',#2784,#2785,#1758,.T.);
#3301=EDGE_CURVE('',#2785,#2785,#2473,.T.);
#3302=EDGE_CURVE('',#2786,#2787,#327,.T.);
#3303=EDGE_CURVE('',#2788,#2786,#328,.T.);
#3304=EDGE_CURVE('',#2788,#2789,#1759,.T.);
#3305=EDGE_CURVE('',#2789,#2789,#2474,.T.);
#3306=EDGE_CURVE('',#2790,#2788,#329,.T.);
#3307=EDGE_CURVE('',#2791,#2790,#330,.T.);
#3308=EDGE_CURVE('',#2792,#2791,#331,.T.);
#3309=EDGE_CURVE('',#2787,#2792,#332,.T.);
#3310=EDGE_CURVE('',#2793,#2793,#2475,.T.);
#3311=EDGE_CURVE('',#2793,#2794,#1760,.T.);
#3312=EDGE_CURVE('',#2795,#2794,#333,.T.);
#3313=EDGE_CURVE('',#2796,#2795,#334,.T.);
#3314=EDGE_CURVE('',#2797,#2796,#335,.T.);
#3315=EDGE_CURVE('',#2798,#2797,#336,.T.);
#3316=EDGE_CURVE('',#2799,#2798,#337,.T.);
#3317=EDGE_CURVE('',#2794,#2799,#338,.T.);
#3318=EDGE_CURVE('',#2790,#2799,#1761,.T.);
#3319=EDGE_CURVE('',#2791,#2798,#1762,.T.);
#3320=EDGE_CURVE('',#2788,#2794,#1763,.T.);
#3321=EDGE_CURVE('',#2786,#2795,#1764,.T.);
#3322=EDGE_CURVE('',#2800,#2800,#2476,.F.);
#3323=EDGE_CURVE('',#2800,#2801,#1765,.T.);
#3324=EDGE_CURVE('',#2801,#2801,#2477,.F.);
#3325=EDGE_CURVE('',#2787,#2796,#1766,.T.);
#3326=EDGE_CURVE('',#2792,#2797,#1767,.T.);
#3327=EDGE_CURVE('',#2802,#2802,#2478,.T.);
#3328=EDGE_CURVE('',#2802,#2803,#1768,.T.);
#3329=EDGE_CURVE('',#2803,#2803,#2479,.T.);
#3330=EDGE_CURVE('',#2804,#2804,#2480,.T.);
#3331=EDGE_CURVE('',#2804,#2805,#1769,.T.);
#3332=EDGE_CURVE('',#2805,#2805,#2481,.T.);
#3333=EDGE_CURVE('',#2806,#2806,#2482,.T.);
#3334=EDGE_CURVE('',#2807,#2807,#2483,.T.);
#3335=EDGE_CURVE('',#2807,#2806,#1770,.T.);
#3336=EDGE_CURVE('',#2808,#2808,#2484,.T.);
#3337=EDGE_CURVE('',#2808,#2807,#1771,.T.);
#3338=EDGE_CURVE('',#2809,#2809,#2485,.T.);
#3339=EDGE_CURVE('',#2809,#2808,#1772,.T.);
#3340=EDGE_CURVE('',#2810,#2810,#2486,.T.);
#3341=EDGE_CURVE('',#2811,#2811,#2487,.F.);
#3342=EDGE_CURVE('',#2811,#2810,#1773,.T.);
#3343=EDGE_CURVE('',#2812,#2812,#2488,.F.);
#3344=EDGE_CURVE('',#2812,#2811,#1774,.T.);
#3345=EDGE_CURVE('',#2813,#2813,#2489,.T.);
#3346=EDGE_CURVE('',#2813,#2812,#1775,.T.);
#3347=EDGE_CURVE('',#2814,#2815,#1776,.T.);
#3348=EDGE_CURVE('',#2815,#2816,#1777,.T.);
#3349=EDGE_CURVE('',#2816,#2817,#1778,.T.);
#3350=EDGE_CURVE('',#2814,#2817,#1779,.T.);
#3351=EDGE_CURVE('',#2815,#2818,#1780,.T.);
#3352=EDGE_CURVE('',#2818,#2819,#1781,.T.);
#3353=EDGE_CURVE('',#2819,#2816,#1782,.T.);
#3354=EDGE_CURVE('',#2818,#2820,#1783,.T.);
#3355=EDGE_CURVE('',#2820,#2821,#1784,.T.);
#3356=EDGE_CURVE('',#2821,#2819,#1785,.T.);
#3357=EDGE_CURVE('',#2820,#2822,#1786,.T.);
#3358=EDGE_CURVE('',#2822,#2823,#1787,.T.);
#3359=EDGE_CURVE('',#2823,#2821,#1788,.T.);
#3360=EDGE_CURVE('',#2822,#2824,#1789,.T.);
#3361=EDGE_CURVE('',#2824,#2825,#1790,.T.);
#3362=EDGE_CURVE('',#2825,#2823,#1791,.T.);
#3363=EDGE_CURVE('',#2824,#2814,#1792,.T.);
#3364=EDGE_CURVE('',#2817,#2825,#1793,.T.);
#3365=EDGE_CURVE('',#2826,#2826,#2490,.T.);
#3366=EDGE_CURVE('',#2826,#2827,#1794,.T.);
#3367=EDGE_CURVE('',#2827,#2827,#2491,.T.);
#3368=EDGE_CURVE('',#2828,#2828,#2492,.T.);
#3369=EDGE_CURVE('',#2828,#2829,#1795,.T.);
#3370=EDGE_CURVE('',#2829,#2829,#2493,.T.);
#3371=EDGE_CURVE('',#2830,#2830,#2494,.T.);
#3372=EDGE_CURVE('',#2830,#2831,#1796,.T.);
#3373=EDGE_CURVE('',#2831,#2831,#2495,.T.);
#3374=EDGE_CURVE('',#2832,#2833,#1797,.T.);
#3375=EDGE_CURVE('',#2834,#2832,#2496,.T.);
#3376=EDGE_CURVE('',#2835,#2834,#1798,.T.);
#3377=EDGE_CURVE('',#2833,#2835,#2497,.T.);
#3378=EDGE_CURVE('',#2836,#2836,#2498,.T.);
#3379=EDGE_CURVE('',#2836,#2837,#1799,.T.);
#3380=EDGE_CURVE('',#2834,#2837,#11,.T.);
#3381=EDGE_CURVE('',#2838,#2832,#12,.T.);
#3382=EDGE_CURVE('',#2838,#2839,#2499,.T.);
#3383=EDGE_CURVE('',#2837,#2839,#13,.T.);
#3384=EDGE_CURVE('',#2840,#2838,#1800,.T.);
#3385=EDGE_CURVE('',#2841,#2840,#2500,.T.);
#3386=EDGE_CURVE('',#2839,#2841,#1801,.T.);
#3387=EDGE_CURVE('',#2842,#2832,#2501,.T.);
#3388=EDGE_CURVE('',#2842,#2843,#1802,.T.);
#3389=EDGE_CURVE('',#2843,#2843,#2502,.T.);
#3390=EDGE_CURVE('',#2838,#2842,#2503,.T.);
#3391=EDGE_CURVE('',#2844,#2835,#14,.T.);
#3392=EDGE_CURVE('',#2833,#2844,#15,.T.);
#3393=EDGE_CURVE('',#2840,#2833,#2504,.T.);
#3394=EDGE_CURVE('',#2845,#2840,#16,.T.);
#3395=EDGE_CURVE('',#2841,#2845,#17,.T.);
#3396=EDGE_CURVE('',#2835,#2841,#2505,.T.);
#3397=EDGE_CURVE('',#2846,#2834,#2506,.T.);
#3398=EDGE_CURVE('',#2839,#2846,#2507,.T.);
#3399=EDGE_CURVE('',#2847,#2847,#2508,.T.);
#3400=EDGE_CURVE('',#2847,#2846,#1803,.T.);
#3401=EDGE_CURVE('',#2844,#2848,#18,.T.);
#3402=EDGE_CURVE('',#2848,#2849,#1804,.T.);
#3403=EDGE_CURVE('',#2849,#2844,#19,.T.);
#3404=EDGE_CURVE('',#2845,#2850,#20,.T.);
#3405=EDGE_CURVE('',#2850,#2851,#1805,.T.);
#3406=EDGE_CURVE('',#2851,#2845,#21,.T.);
#3407=EDGE_CURVE('',#2851,#2850,#2509,.T.);
#3408=EDGE_CURVE('',#2849,#2848,#2510,.T.);
#3409=EDGE_CURVE('',#2852,#2853,#22,.T.);
#3410=EDGE_CURVE('',#2854,#2852,#23,.T.);
#3411=EDGE_CURVE('',#2854,#2855,#1806,.T.);
#3412=EDGE_CURVE('',#2855,#2855,#2511,.T.);
#3413=EDGE_CURVE('',#2853,#2854,#24,.T.);
#3414=EDGE_CURVE('',#2856,#2856,#2512,.T.);
#3415=EDGE_CURVE('',#2856,#2852,#1807,.T.);
#3416=EDGE_CURVE('',#2852,#2857,#1808,.T.);
#3417=EDGE_CURVE('',#2857,#2857,#2513,.T.);
#3418=EDGE_CURVE('',#2858,#2858,#2514,.T.);
#3419=EDGE_CURVE('',#2858,#2859,#1809,.T.);
#3420=EDGE_CURVE('',#2859,#2859,#2515,.T.);
#3421=EDGE_CURVE('',#2860,#2860,#2516,.T.);
#3422=EDGE_CURVE('',#2860,#2861,#1810,.T.);
#3423=EDGE_CURVE('',#2861,#2861,#2517,.T.);
#3424=EDGE_CURVE('',#2862,#2862,#2518,.T.);
#3425=EDGE_CURVE('',#2862,#2863,#1811,.T.);
#3426=EDGE_CURVE('',#2863,#2863,#2519,.T.);
#3427=EDGE_CURVE('',#2864,#2864,#2520,.T.);
#3428=EDGE_CURVE('',#2864,#2865,#1812,.T.);
#3429=EDGE_CURVE('',#2865,#2865,#2521,.T.);
#3430=EDGE_CURVE('',#2866,#2866,#2522,.T.);
#3431=EDGE_CURVE('',#2866,#2867,#1813,.T.);
#3432=EDGE_CURVE('',#2867,#2867,#2523,.T.);
#3433=EDGE_CURVE('',#2868,#2868,#2524,.T.);
#3434=EDGE_CURVE('',#2868,#2869,#1814,.T.);
#3435=EDGE_CURVE('',#2869,#2869,#2525,.T.);
#3436=EDGE_CURVE('',#2870,#2871,#25,.T.);
#3437=EDGE_CURVE('',#2872,#2870,#2526,.T.);
#3438=EDGE_CURVE('',#2872,#2873,#1815,.T.);
#3439=EDGE_CURVE('',#2873,#2873,#2527,.T.);
#3440=EDGE_CURVE('',#2871,#2872,#2528,.T.);
#3441=EDGE_CURVE('',#2874,#2875,#2529,.T.);
#3442=EDGE_CURVE('',#2870,#2876,#2530,.T.);
#3443=EDGE_CURVE('',#2876,#2871,#2531,.T.);
#3444=EDGE_CURVE('',#2876,#2877,#1816,.T.);
#3445=EDGE_CURVE('',#2877,#2877,#2532,.T.);
#3446=EDGE_CURVE('',#2878,#2878,#2533,.T.);
#3447=EDGE_CURVE('',#2879,#2879,#2534,.T.);
#3448=EDGE_CURVE('',#2879,#2878,#1817,.T.);
#3449=EDGE_CURVE('',#2880,#2880,#2535,.T.);
#3450=EDGE_CURVE('',#2880,#2881,#1818,.T.);
#3451=EDGE_CURVE('',#2881,#2881,#2536,.T.);
#3452=EDGE_CURVE('',#2882,#2883,#2537,.T.);
#3453=EDGE_CURVE('',#2883,#2884,#2538,.T.);
#3454=EDGE_CURVE('',#2885,#2884,#2539,.T.);
#3455=EDGE_CURVE('',#2882,#2885,#2540,.T.);
#3456=EDGE_CURVE('',#2884,#2882,#26,.T.);
#3457=EDGE_CURVE('',#2883,#2886,#1819,.T.);
#3458=EDGE_CURVE('',#2886,#2886,#2541,.T.);
#3459=EDGE_CURVE('',#2887,#2887,#2542,.T.);
#3460=EDGE_CURVE('',#2888,#2888,#2543,.T.);
#3461=EDGE_CURVE('',#2888,#2887,#1820,.T.);
#3462=EDGE_CURVE('',#2889,#2889,#2544,.T.);
#3463=EDGE_CURVE('',#2890,#2890,#2545,.T.);
#3464=EDGE_CURVE('',#2891,#2891,#2546,.T.);
#3465=EDGE_CURVE('',#2891,#2889,#1821,.T.);
#3466=EDGE_CURVE('',#2890,#2885,#1822,.T.);
#3467=EDGE_CURVE('',#2892,#2893,#1823,.T.);
#3468=EDGE_CURVE('',#2893,#2894,#1824,.T.);
#3469=EDGE_CURVE('',#2894,#2895,#1825,.T.);
#3470=EDGE_CURVE('',#2895,#2896,#1826,.T.);
#3471=EDGE_CURVE('',#2896,#2897,#1827,.T.);
#3472=EDGE_CURVE('',#2897,#2892,#1828,.T.);
#3473=EDGE_CURVE('',#2898,#2898,#2547,.T.);
#3474=EDGE_CURVE('',#2899,#2900,#1829,.T.);
#3475=EDGE_CURVE('',#2900,#2901,#1830,.T.);
#3476=EDGE_CURVE('',#2901,#2902,#1831,.T.);
#3477=EDGE_CURVE('',#2902,#2903,#1832,.T.);
#3478=EDGE_CURVE('',#2903,#2904,#1833,.T.);
#3479=EDGE_CURVE('',#2904,#2899,#1834,.T.);
#3480=EDGE_CURVE('',#2905,#2905,#2548,.T.);
#3481=EDGE_CURVE('',#2899,#2893,#1835,.T.);
#3482=EDGE_CURVE('',#2894,#2904,#1836,.T.);
#3483=EDGE_CURVE('',#2895,#2903,#1837,.T.);
#3484=EDGE_CURVE('',#2896,#2902,#1838,.T.);
#3485=EDGE_CURVE('',#2897,#2901,#1839,.T.);
#3486=EDGE_CURVE('',#2892,#2900,#1840,.T.);
#3487=EDGE_CURVE('',#2905,#2906,#1841,.T.);
#3488=EDGE_CURVE('',#2906,#2906,#2549,.T.);
#3489=EDGE_CURVE('',#2907,#2907,#2550,.T.);
#3490=EDGE_CURVE('',#2908,#2908,#2551,.T.);
#3491=EDGE_CURVE('',#2906,#2907,#1842,.T.);
#3492=EDGE_CURVE('',#2909,#2909,#2552,.T.);
#3493=EDGE_CURVE('',#2909,#2898,#1843,.T.);
#3494=EDGE_CURVE('',#2910,#2910,#2553,.T.);
#3495=EDGE_CURVE('',#2910,#2909,#1844,.T.);
#3496=EDGE_CURVE('',#2911,#2911,#2554,.T.);
#3497=EDGE_CURVE('',#2911,#2908,#1845,.T.);
#3498=EDGE_CURVE('',#2912,#2912,#2555,.T.);
#3499=EDGE_CURVE('',#2912,#2913,#1846,.T.);
#3500=EDGE_CURVE('',#2913,#2913,#2556,.T.);
#3501=EDGE_CURVE('',#2914,#2914,#2557,.T.);
#3502=EDGE_CURVE('',#2914,#2915,#1847,.T.);
#3503=EDGE_CURVE('',#2915,#2915,#2558,.T.);
#3504=EDGE_CURVE('',#2916,#2916,#2559,.T.);
#3505=EDGE_CURVE('',#2916,#2917,#1848,.T.);
#3506=EDGE_CURVE('',#2917,#2917,#2560,.T.);
#3507=EDGE_CURVE('',#2918,#2918,#2561,.T.);
#3508=EDGE_CURVE('',#2918,#2919,#1849,.T.);
#3509=EDGE_CURVE('',#2919,#2919,#2562,.T.);
#3510=EDGE_CURVE('',#2920,#2920,#2563,.T.);
#3511=EDGE_CURVE('',#2921,#2921,#2564,.T.);
#3512=EDGE_CURVE('',#2922,#2922,#2565,.T.);
#3513=EDGE_CURVE('',#2922,#2920,#1850,.T.);
#3514=EDGE_CURVE('',#2923,#2923,#2566,.T.);
#3515=EDGE_CURVE('',#2923,#2924,#1851,.T.);
#3516=EDGE_CURVE('',#2924,#2924,#2567,.T.);
#3517=EDGE_CURVE('',#2921,#2925,#1852,.T.);
#3518=EDGE_CURVE('',#2925,#2925,#2568,.T.);
#3519=EDGE_CURVE('',#2926,#2926,#2569,.T.);
#3520=EDGE_CURVE('',#2926,#2927,#1853,.T.);
#3521=EDGE_CURVE('',#2927,#2927,#2570,.T.);
#3522=EDGE_CURVE('',#2928,#2928,#2571,.T.);
#3523=EDGE_CURVE('',#2928,#2929,#1854,.T.);
#3524=EDGE_CURVE('',#2929,#2929,#2572,.T.);
#3525=EDGE_CURVE('',#2930,#2930,#2573,.T.);
#3526=EDGE_CURVE('',#2930,#2931,#1855,.T.);
#3527=EDGE_CURVE('',#2931,#2931,#2574,.T.);
#3528=EDGE_CURVE('',#2932,#2932,#2575,.T.);
#3529=EDGE_CURVE('',#2932,#2933,#1856,.T.);
#3530=EDGE_CURVE('',#2933,#2933,#2576,.T.);
#3531=EDGE_CURVE('',#2934,#2934,#2577,.T.);
#3532=EDGE_CURVE('',#2935,#2935,#2578,.T.);
#3533=EDGE_CURVE('',#2934,#2936,#1857,.T.);
#3534=EDGE_CURVE('',#2936,#2936,#2579,.T.);
#3535=EDGE_CURVE('',#2937,#2937,#2580,.T.);
#3536=EDGE_CURVE('',#2937,#2938,#1858,.T.);
#3537=EDGE_CURVE('',#2938,#2938,#2581,.T.);
#3538=EDGE_CURVE('',#2939,#2939,#2582,.T.);
#3539=EDGE_CURVE('',#2939,#2935,#1859,.T.);
#3540=EDGE_CURVE('',#2940,#2940,#2583,.T.);
#3541=EDGE_CURVE('',#2941,#2941,#2584,.T.);
#3542=EDGE_CURVE('',#2941,#2940,#1860,.T.);
#3543=EDGE_CURVE('',#2942,#2942,#2585,.T.);
#3544=EDGE_CURVE('',#2942,#2941,#1861,.T.);
#3545=EDGE_CURVE('',#2943,#2943,#2586,.T.);
#3546=EDGE_CURVE('',#2943,#2942,#1862,.T.);
#3547=EDGE_CURVE('',#2944,#2944,#2587,.T.);
#3548=EDGE_CURVE('',#2945,#2945,#2588,.F.);
#3549=EDGE_CURVE('',#2945,#2944,#1863,.T.);
#3550=EDGE_CURVE('',#2946,#2946,#2589,.F.);
#3551=EDGE_CURVE('',#2946,#2945,#1864,.T.);
#3552=EDGE_CURVE('',#2947,#2947,#2590,.T.);
#3553=EDGE_CURVE('',#2947,#2946,#1865,.T.);
#3554=EDGE_CURVE('',#2948,#2949,#1866,.T.);
#3555=EDGE_CURVE('',#2949,#2950,#1867,.T.);
#3556=EDGE_CURVE('',#2950,#2951,#1868,.T.);
#3557=EDGE_CURVE('',#2948,#2951,#1869,.T.);
#3558=EDGE_CURVE('',#2949,#2952,#1870,.T.);
#3559=EDGE_CURVE('',#2952,#2953,#1871,.T.);
#3560=EDGE_CURVE('',#2953,#2950,#1872,.T.);
#3561=EDGE_CURVE('',#2952,#2954,#1873,.T.);
#3562=EDGE_CURVE('',#2954,#2955,#1874,.T.);
#3563=EDGE_CURVE('',#2955,#2953,#1875,.T.);
#3564=EDGE_CURVE('',#2954,#2956,#1876,.T.);
#3565=EDGE_CURVE('',#2956,#2957,#1877,.T.);
#3566=EDGE_CURVE('',#2957,#2955,#1878,.T.);
#3567=EDGE_CURVE('',#2956,#2958,#1879,.T.);
#3568=EDGE_CURVE('',#2958,#2959,#1880,.T.);
#3569=EDGE_CURVE('',#2959,#2957,#1881,.T.);
#3570=EDGE_CURVE('',#2958,#2948,#1882,.T.);
#3571=EDGE_CURVE('',#2951,#2959,#1883,.T.);
#3572=EDGE_CURVE('',#2960,#2960,#2591,.T.);
#3573=EDGE_CURVE('',#2960,#2961,#1884,.T.);
#3574=EDGE_CURVE('',#2961,#2961,#2592,.T.);
#3575=EDGE_CURVE('',#2962,#2962,#2593,.T.);
#3576=EDGE_CURVE('',#2962,#2963,#1885,.T.);
#3577=EDGE_CURVE('',#2963,#2963,#2594,.T.);
#3578=EDGE_CURVE('',#2964,#2965,#339,.T.);
#3579=EDGE_CURVE('',#2966,#2964,#340,.T.);
#3580=EDGE_CURVE('',#2966,#2967,#1886,.T.);
#3581=EDGE_CURVE('',#2967,#2967,#2595,.T.);
#3582=EDGE_CURVE('',#2968,#2966,#341,.T.);
#3583=EDGE_CURVE('',#2969,#2968,#342,.T.);
#3584=EDGE_CURVE('',#2970,#2969,#343,.T.);
#3585=EDGE_CURVE('',#2965,#2970,#344,.T.);
#3586=EDGE_CURVE('',#2971,#2971,#2596,.T.);
#3587=EDGE_CURVE('',#2971,#2972,#1887,.T.);
#3588=EDGE_CURVE('',#2973,#2972,#345,.T.);
#3589=EDGE_CURVE('',#2974,#2973,#346,.T.);
#3590=EDGE_CURVE('',#2975,#2974,#347,.T.);
#3591=EDGE_CURVE('',#2976,#2975,#348,.T.);
#3592=EDGE_CURVE('',#2977,#2976,#349,.T.);
#3593=EDGE_CURVE('',#2972,#2977,#350,.T.);
#3594=EDGE_CURVE('',#2968,#2977,#1888,.T.);
#3595=EDGE_CURVE('',#2969,#2976,#1889,.T.);
#3596=EDGE_CURVE('',#2966,#2972,#1890,.T.);
#3597=EDGE_CURVE('',#2964,#2973,#1891,.T.);
#3598=EDGE_CURVE('',#2978,#2978,#2597,.F.);
#3599=EDGE_CURVE('',#2978,#2979,#1892,.T.);
#3600=EDGE_CURVE('',#2979,#2979,#2598,.F.);
#3601=EDGE_CURVE('',#2965,#2974,#1893,.T.);
#3602=EDGE_CURVE('',#2970,#2975,#1894,.T.);
#3603=EDGE_CURVE('',#2980,#2981,#2599,.T.);
#3604=EDGE_CURVE('',#2982,#2980,#1895,.T.);
#3605=EDGE_CURVE('',#2983,#2982,#1896,.T.);
#3606=EDGE_CURVE('',#2983,#2981,#1897,.T.);
#3607=EDGE_CURVE('',#2981,#2984,#2600,.T.);
#3608=EDGE_CURVE('',#2985,#2983,#1898,.T.);
#3609=EDGE_CURVE('',#2985,#2986,#1899,.T.);
#3610=EDGE_CURVE('',#2984,#2986,#2601,.T.);
#3611=EDGE_CURVE('',#2986,#2987,#2602,.T.);
#3612=EDGE_CURVE('',#2988,#2985,#1900,.T.);
#3613=EDGE_CURVE('',#2988,#2987,#1901,.T.);
#3614=EDGE_CURVE('',#2987,#2980,#2603,.T.);
#3615=EDGE_CURVE('',#2982,#2988,#1902,.T.);
#3616=EDGE_CURVE('',#2989,#2989,#2604,.T.);
#3617=EDGE_CURVE('',#2989,#2990,#1903,.T.);
#3618=EDGE_CURVE('',#2990,#2990,#2605,.T.);
#3619=EDGE_CURVE('',#2984,#2991,#2606,.T.);
#3620=EDGE_CURVE('',#2992,#2992,#2607,.T.);
#3621=EDGE_CURVE('',#2992,#2993,#1904,.T.);
#3622=EDGE_CURVE('',#2993,#2993,#2608,.T.);
#3623=EDGE_CURVE('',#2994,#2995,#2609,.T.);
#3624=EDGE_CURVE('',#2996,#2995,#1905,.T.);
#3625=EDGE_CURVE('',#2994,#2996,#1906,.T.);
#3626=EDGE_CURVE('',#2997,#2998,#2610,.T.);
#3627=EDGE_CURVE('',#2999,#2998,#1907,.T.);
#3628=EDGE_CURVE('',#2997,#2999,#1908,.T.);
#3629=EDGE_CURVE('',#3000,#3001,#2611,.T.);
#3630=EDGE_CURVE('',#3002,#3001,#1909,.T.);
#3631=EDGE_CURVE('',#3000,#3002,#1910,.T.);
#3632=EDGE_CURVE('',#3003,#3004,#2612,.T.);
#3633=EDGE_CURVE('',#3005,#3004,#1911,.T.);
#3634=EDGE_CURVE('',#3003,#3005,#1912,.T.);
#3635=EDGE_CURVE('',#2994,#3004,#1913,.T.);
#3636=EDGE_CURVE('',#2996,#3006,#1914,.T.);
#3637=EDGE_CURVE('',#3007,#3006,#1915,.T.);
#3638=EDGE_CURVE('',#3005,#3007,#1916,.T.);
#3639=EDGE_CURVE('',#3003,#3001,#1917,.T.);
#3640=EDGE_CURVE('',#3008,#3007,#1918,.T.);
#3641=EDGE_CURVE('',#3002,#3008,#1919,.T.);
#3642=EDGE_CURVE('',#3000,#2998,#1920,.T.);
#3643=EDGE_CURVE('',#3009,#3008,#1921,.T.);
#3644=EDGE_CURVE('',#2999,#3009,#1922,.T.);
#3645=EDGE_CURVE('',#2997,#2995,#1923,.T.);
#3646=EDGE_CURVE('',#3006,#3009,#1924,.T.);
#3647=EDGE_CURVE('',#2998,#3000,#2613,.T.);
#3648=EDGE_CURVE('',#2995,#3010,#2614,.T.);
#3649=EDGE_CURVE('',#3010,#2997,#2615,.T.);
#3650=EDGE_CURVE('',#3004,#2994,#2616,.T.);
#3651=EDGE_CURVE('',#3001,#3003,#2617,.T.);
#3652=EDGE_CURVE('',#3011,#3012,#1925,.T.);
#3653=EDGE_CURVE('',#3012,#3013,#1926,.T.);
#3654=EDGE_CURVE('',#3014,#3013,#1927,.T.);
#3655=EDGE_CURVE('',#3011,#3014,#1928,.T.);
#3656=EDGE_CURVE('',#3015,#3011,#1929,.T.);
#3657=EDGE_CURVE('',#3016,#3014,#1930,.T.);
#3658=EDGE_CURVE('',#3015,#3016,#1931,.T.);
#3659=EDGE_CURVE('',#3017,#3015,#1932,.T.);
#3660=EDGE_CURVE('',#3018,#3016,#1933,.T.);
#3661=EDGE_CURVE('',#3017,#3018,#1934,.T.);
#3662=EDGE_CURVE('',#3012,#3017,#1935,.T.);
#3663=EDGE_CURVE('',#3013,#3018,#1936,.T.);
#3664=EDGE_CURVE('',#3010,#3019,#1937,.T.);
#3665=EDGE_CURVE('',#3019,#3019,#2618,.T.);
#3666=EDGE_CURVE('',#3020,#3021,#1938,.T.);
#3667=EDGE_CURVE('',#3022,#3020,#1939,.T.);
#3668=EDGE_CURVE('',#3023,#3022,#1940,.T.);
#3669=EDGE_CURVE('',#3023,#3021,#1941,.T.);
#3670=EDGE_CURVE('',#3021,#3024,#1942,.T.);
#3671=EDGE_CURVE('',#3025,#3023,#1943,.T.);
#3672=EDGE_CURVE('',#3025,#3024,#1944,.T.);
#3673=EDGE_CURVE('',#3024,#3026,#1945,.T.);
#3674=EDGE_CURVE('',#3027,#3025,#1946,.T.);
#3675=EDGE_CURVE('',#3027,#3026,#1947,.T.);
#3676=EDGE_CURVE('',#3026,#3020,#1948,.T.);
#3677=EDGE_CURVE('',#3022,#3027,#1949,.T.);
#3678=EDGE_CURVE('',#3028,#3029,#1950,.T.);
#3679=EDGE_CURVE('',#3029,#3030,#1951,.T.);
#3680=EDGE_CURVE('',#3031,#3030,#1952,.T.);
#3681=EDGE_CURVE('',#3028,#3031,#1953,.T.);
#3682=EDGE_CURVE('',#3032,#3028,#1954,.T.);
#3683=EDGE_CURVE('',#3033,#3031,#1955,.T.);
#3684=EDGE_CURVE('',#3032,#3033,#1956,.T.);
#3685=EDGE_CURVE('',#3034,#3032,#1957,.T.);
#3686=EDGE_CURVE('',#3035,#3033,#1958,.T.);
#3687=EDGE_CURVE('',#3034,#3035,#1959,.T.);
#3688=EDGE_CURVE('',#3029,#3034,#1960,.T.);
#3689=EDGE_CURVE('',#3030,#3035,#1961,.T.);
#3690=EDGE_CURVE('',#3036,#3036,#2619,.T.);
#3691=EDGE_CURVE('',#3036,#3037,#1962,.T.);
#3692=EDGE_CURVE('',#3037,#3037,#2620,.T.);
#3693=EDGE_CURVE('',#3038,#3038,#2621,.T.);
#3694=EDGE_CURVE('',#3038,#3039,#1963,.T.);
#3695=EDGE_CURVE('',#3039,#3039,#2622,.T.);
#3696=EDGE_CURVE('',#3040,#3041,#1964,.T.);
#3697=EDGE_CURVE('',#3041,#3042,#1965,.T.);
#3698=EDGE_CURVE('',#3043,#3042,#1966,.T.);
#3699=EDGE_CURVE('',#3040,#3043,#1967,.T.);
#3700=EDGE_CURVE('',#3044,#3040,#1968,.T.);
#3701=EDGE_CURVE('',#3045,#3043,#1969,.T.);
#3702=EDGE_CURVE('',#3044,#3045,#1970,.T.);
#3703=EDGE_CURVE('',#3046,#3044,#1971,.T.);
#3704=EDGE_CURVE('',#3047,#3045,#1972,.T.);
#3705=EDGE_CURVE('',#3046,#3047,#1973,.T.);
#3706=EDGE_CURVE('',#3041,#3046,#1974,.T.);
#3707=EDGE_CURVE('',#3042,#3047,#1975,.T.);
#3708=EDGE_CURVE('',#3048,#3049,#1976,.T.);
#3709=EDGE_CURVE('',#3049,#3050,#1977,.T.);
#3710=EDGE_CURVE('',#3050,#3051,#1978,.T.);
#3711=EDGE_CURVE('',#3048,#3051,#1979,.T.);
#3712=EDGE_CURVE('',#3049,#3052,#1980,.T.);
#3713=EDGE_CURVE('',#3052,#3053,#1981,.T.);
#3714=EDGE_CURVE('',#3053,#3050,#1982,.T.);
#3715=EDGE_CURVE('',#3052,#3054,#1983,.T.);
#3716=EDGE_CURVE('',#3054,#3055,#1984,.T.);
#3717=EDGE_CURVE('',#3055,#3053,#1985,.T.);
#3718=EDGE_CURVE('',#3054,#3056,#1986,.T.);
#3719=EDGE_CURVE('',#3056,#3057,#1987,.T.);
#3720=EDGE_CURVE('',#3057,#3055,#1988,.T.);
#3721=EDGE_CURVE('',#3056,#3058,#1989,.T.);
#3722=EDGE_CURVE('',#3058,#3059,#1990,.T.);
#3723=EDGE_CURVE('',#3059,#3057,#1991,.T.);
#3724=EDGE_CURVE('',#3058,#3048,#1992,.T.);
#3725=EDGE_CURVE('',#3051,#3059,#1993,.T.);
#3726=EDGE_CURVE('',#3060,#3060,#2623,.T.);
#3727=EDGE_CURVE('',#3061,#3061,#2624,.T.);
#3728=EDGE_CURVE('',#3062,#3062,#2625,.T.);
#3729=EDGE_CURVE('',#3062,#3061,#1994,.T.);
#3730=EDGE_CURVE('',#3063,#3063,#2626,.T.);
#3731=EDGE_CURVE('',#3063,#3062,#1995,.T.);
#3732=EDGE_CURVE('',#3064,#3064,#2627,.T.);
#3733=EDGE_CURVE('',#3064,#3063,#1996,.T.);
#3734=EDGE_CURVE('',#3065,#3065,#2628,.T.);
#3735=EDGE_CURVE('',#3066,#3066,#2629,.F.);
#3736=EDGE_CURVE('',#3066,#3065,#1997,.T.);
#3737=EDGE_CURVE('',#3060,#3066,#1998,.T.);
#3738=ORIENTED_EDGE('',*,*,#3067,.F.);
#3739=ORIENTED_EDGE('',*,*,#3068,.T.);
#3740=ORIENTED_EDGE('',*,*,#3069,.F.);
#3741=ORIENTED_EDGE('',*,*,#3068,.F.);
#3742=ORIENTED_EDGE('',*,*,#3067,.T.);
#3743=ORIENTED_EDGE('',*,*,#3070,.F.);
#3744=ORIENTED_EDGE('',*,*,#3071,.T.);
#3745=ORIENTED_EDGE('',*,*,#3072,.F.);
#3746=ORIENTED_EDGE('',*,*,#3071,.F.);
#3747=ORIENTED_EDGE('',*,*,#3070,.T.);
#3748=ORIENTED_EDGE('',*,*,#3073,.F.);
#3749=ORIENTED_EDGE('',*,*,#3074,.T.);
#3750=ORIENTED_EDGE('',*,*,#3075,.F.);
#3751=ORIENTED_EDGE('',*,*,#3074,.F.);
#3752=ORIENTED_EDGE('',*,*,#3076,.F.);
#3753=ORIENTED_EDGE('',*,*,#3077,.T.);
#3754=ORIENTED_EDGE('',*,*,#3078,.F.);
#3755=ORIENTED_EDGE('',*,*,#3077,.F.);
#3756=ORIENTED_EDGE('',*,*,#3079,.F.);
#3757=ORIENTED_EDGE('',*,*,#3080,.T.);
#3758=ORIENTED_EDGE('',*,*,#3081,.F.);
#3759=ORIENTED_EDGE('',*,*,#3080,.F.);
#3760=ORIENTED_EDGE('',*,*,#3082,.F.);
#3761=ORIENTED_EDGE('',*,*,#3083,.T.);
#3762=ORIENTED_EDGE('',*,*,#3084,.F.);
#3763=ORIENTED_EDGE('',*,*,#3083,.F.);
#3764=ORIENTED_EDGE('',*,*,#3085,.F.);
#3765=ORIENTED_EDGE('',*,*,#3086,.F.);
#3766=ORIENTED_EDGE('',*,*,#3087,.F.);
#3767=ORIENTED_EDGE('',*,*,#3088,.F.);
#3768=ORIENTED_EDGE('',*,*,#3089,.F.);
#3769=ORIENTED_EDGE('',*,*,#3090,.F.);
#3770=ORIENTED_EDGE('',*,*,#3091,.F.);
#3771=ORIENTED_EDGE('',*,*,#3086,.T.);
#3772=ORIENTED_EDGE('',*,*,#3088,.T.);
#3773=ORIENTED_EDGE('',*,*,#3092,.T.);
#3774=ORIENTED_EDGE('',*,*,#3093,.T.);
#3775=ORIENTED_EDGE('',*,*,#3094,.T.);
#3776=ORIENTED_EDGE('',*,*,#3095,.T.);
#3777=ORIENTED_EDGE('',*,*,#3096,.T.);
#3778=ORIENTED_EDGE('',*,*,#3069,.T.);
#3779=ORIENTED_EDGE('',*,*,#3072,.T.);
#3780=ORIENTED_EDGE('',*,*,#3097,.F.);
#3781=ORIENTED_EDGE('',*,*,#3098,.T.);
#3782=ORIENTED_EDGE('',*,*,#3099,.F.);
#3783=ORIENTED_EDGE('',*,*,#3098,.F.);
#3784=ORIENTED_EDGE('',*,*,#3100,.F.);
#3785=ORIENTED_EDGE('',*,*,#3101,.T.);
#3786=ORIENTED_EDGE('',*,*,#3102,.T.);
#3787=ORIENTED_EDGE('',*,*,#3101,.F.);
#3788=ORIENTED_EDGE('',*,*,#3102,.F.);
#3789=ORIENTED_EDGE('',*,*,#3103,.F.);
#3790=ORIENTED_EDGE('',*,*,#3100,.T.);
#3791=ORIENTED_EDGE('',*,*,#3099,.T.);
#3792=ORIENTED_EDGE('',*,*,#3090,.T.);
#3793=ORIENTED_EDGE('',*,*,#3104,.F.);
#3794=ORIENTED_EDGE('',*,*,#3103,.T.);
#3795=ORIENTED_EDGE('',*,*,#3085,.T.);
#3796=ORIENTED_EDGE('',*,*,#3096,.F.);
#3797=ORIENTED_EDGE('',*,*,#3105,.F.);
#3798=ORIENTED_EDGE('',*,*,#3106,.T.);
#3799=ORIENTED_EDGE('',*,*,#3107,.T.);
#3800=ORIENTED_EDGE('',*,*,#3092,.F.);
#3801=ORIENTED_EDGE('',*,*,#3087,.T.);
#3802=ORIENTED_EDGE('',*,*,#3091,.T.);
#3803=ORIENTED_EDGE('',*,*,#3104,.T.);
#3804=ORIENTED_EDGE('',*,*,#3089,.T.);
#3805=ORIENTED_EDGE('',*,*,#3075,.T.);
#3806=ORIENTED_EDGE('',*,*,#3078,.T.);
#3807=ORIENTED_EDGE('',*,*,#3081,.T.);
#3808=ORIENTED_EDGE('',*,*,#3084,.T.);
#3809=ORIENTED_EDGE('',*,*,#3108,.T.);
#3810=ORIENTED_EDGE('',*,*,#3105,.T.);
#3811=ORIENTED_EDGE('',*,*,#3095,.F.);
#3812=ORIENTED_EDGE('',*,*,#3109,.F.);
#3813=ORIENTED_EDGE('',*,*,#3110,.T.);
#3814=ORIENTED_EDGE('',*,*,#3109,.T.);
#3815=ORIENTED_EDGE('',*,*,#3094,.F.);
#3816=ORIENTED_EDGE('',*,*,#3111,.F.);
#3817=ORIENTED_EDGE('',*,*,#3097,.T.);
#3818=ORIENTED_EDGE('',*,*,#3082,.T.);
#3819=ORIENTED_EDGE('',*,*,#3079,.T.);
#3820=ORIENTED_EDGE('',*,*,#3076,.T.);
#3821=ORIENTED_EDGE('',*,*,#3073,.T.);
#3822=ORIENTED_EDGE('',*,*,#3112,.T.);
#3823=ORIENTED_EDGE('',*,*,#3111,.T.);
#3824=ORIENTED_EDGE('',*,*,#3093,.F.);
#3825=ORIENTED_EDGE('',*,*,#3107,.F.);
#3826=ORIENTED_EDGE('',*,*,#3112,.F.);
#3827=ORIENTED_EDGE('',*,*,#3106,.F.);
#3828=ORIENTED_EDGE('',*,*,#3108,.F.);
#3829=ORIENTED_EDGE('',*,*,#3110,.F.);
#3830=ORIENTED_EDGE('',*,*,#3113,.F.);
#3831=ORIENTED_EDGE('',*,*,#3114,.T.);
#3832=ORIENTED_EDGE('',*,*,#3115,.F.);
#3833=ORIENTED_EDGE('',*,*,#3114,.F.);
#3834=ORIENTED_EDGE('',*,*,#3113,.T.);
#3835=ORIENTED_EDGE('',*,*,#3116,.F.);
#3836=ORIENTED_EDGE('',*,*,#3117,.T.);
#3837=ORIENTED_EDGE('',*,*,#3118,.F.);
#3838=ORIENTED_EDGE('',*,*,#3117,.F.);
#3839=ORIENTED_EDGE('',*,*,#3116,.T.);
#3840=ORIENTED_EDGE('',*,*,#3119,.F.);
#3841=ORIENTED_EDGE('',*,*,#3120,.T.);
#3842=ORIENTED_EDGE('',*,*,#3121,.F.);
#3843=ORIENTED_EDGE('',*,*,#3120,.F.);
#3844=ORIENTED_EDGE('',*,*,#3122,.F.);
#3845=ORIENTED_EDGE('',*,*,#3123,.T.);
#3846=ORIENTED_EDGE('',*,*,#3124,.F.);
#3847=ORIENTED_EDGE('',*,*,#3123,.F.);
#3848=ORIENTED_EDGE('',*,*,#3125,.F.);
#3849=ORIENTED_EDGE('',*,*,#3126,.T.);
#3850=ORIENTED_EDGE('',*,*,#3127,.F.);
#3851=ORIENTED_EDGE('',*,*,#3126,.F.);
#3852=ORIENTED_EDGE('',*,*,#3128,.F.);
#3853=ORIENTED_EDGE('',*,*,#3129,.T.);
#3854=ORIENTED_EDGE('',*,*,#3130,.F.);
#3855=ORIENTED_EDGE('',*,*,#3129,.F.);
#3856=ORIENTED_EDGE('',*,*,#3131,.F.);
#3857=ORIENTED_EDGE('',*,*,#3132,.F.);
#3858=ORIENTED_EDGE('',*,*,#3133,.F.);
#3859=ORIENTED_EDGE('',*,*,#3134,.F.);
#3860=ORIENTED_EDGE('',*,*,#3135,.F.);
#3861=ORIENTED_EDGE('',*,*,#3136,.F.);
#3862=ORIENTED_EDGE('',*,*,#3137,.F.);
#3863=ORIENTED_EDGE('',*,*,#3132,.T.);
#3864=ORIENTED_EDGE('',*,*,#3134,.T.);
#3865=ORIENTED_EDGE('',*,*,#3138,.T.);
#3866=ORIENTED_EDGE('',*,*,#3139,.T.);
#3867=ORIENTED_EDGE('',*,*,#3140,.T.);
#3868=ORIENTED_EDGE('',*,*,#3141,.T.);
#3869=ORIENTED_EDGE('',*,*,#3142,.T.);
#3870=ORIENTED_EDGE('',*,*,#3115,.T.);
#3871=ORIENTED_EDGE('',*,*,#3118,.T.);
#3872=ORIENTED_EDGE('',*,*,#3143,.F.);
#3873=ORIENTED_EDGE('',*,*,#3144,.T.);
#3874=ORIENTED_EDGE('',*,*,#3145,.F.);
#3875=ORIENTED_EDGE('',*,*,#3144,.F.);
#3876=ORIENTED_EDGE('',*,*,#3146,.F.);
#3877=ORIENTED_EDGE('',*,*,#3147,.T.);
#3878=ORIENTED_EDGE('',*,*,#3148,.T.);
#3879=ORIENTED_EDGE('',*,*,#3147,.F.);
#3880=ORIENTED_EDGE('',*,*,#3148,.F.);
#3881=ORIENTED_EDGE('',*,*,#3143,.T.);
#3882=ORIENTED_EDGE('',*,*,#3146,.T.);
#3883=ORIENTED_EDGE('',*,*,#3149,.F.);
#3884=ORIENTED_EDGE('',*,*,#3136,.T.);
#3885=ORIENTED_EDGE('',*,*,#3150,.F.);
#3886=ORIENTED_EDGE('',*,*,#3149,.T.);
#3887=ORIENTED_EDGE('',*,*,#3151,.T.);
#3888=ORIENTED_EDGE('',*,*,#3152,.T.);
#3889=ORIENTED_EDGE('',*,*,#3140,.F.);
#3890=ORIENTED_EDGE('',*,*,#3153,.F.);
#3891=ORIENTED_EDGE('',*,*,#3145,.T.);
#3892=ORIENTED_EDGE('',*,*,#3130,.T.);
#3893=ORIENTED_EDGE('',*,*,#3127,.T.);
#3894=ORIENTED_EDGE('',*,*,#3124,.T.);
#3895=ORIENTED_EDGE('',*,*,#3121,.T.);
#3896=ORIENTED_EDGE('',*,*,#3154,.T.);
#3897=ORIENTED_EDGE('',*,*,#3153,.T.);
#3898=ORIENTED_EDGE('',*,*,#3139,.F.);
#3899=ORIENTED_EDGE('',*,*,#3155,.F.);
#3900=ORIENTED_EDGE('',*,*,#3131,.T.);
#3901=ORIENTED_EDGE('',*,*,#3142,.F.);
#3902=ORIENTED_EDGE('',*,*,#3156,.F.);
#3903=ORIENTED_EDGE('',*,*,#3157,.T.);
#3904=ORIENTED_EDGE('',*,*,#3155,.T.);
#3905=ORIENTED_EDGE('',*,*,#3138,.F.);
#3906=ORIENTED_EDGE('',*,*,#3133,.T.);
#3907=ORIENTED_EDGE('',*,*,#3137,.T.);
#3908=ORIENTED_EDGE('',*,*,#3150,.T.);
#3909=ORIENTED_EDGE('',*,*,#3135,.T.);
#3910=ORIENTED_EDGE('',*,*,#3119,.T.);
#3911=ORIENTED_EDGE('',*,*,#3122,.T.);
#3912=ORIENTED_EDGE('',*,*,#3125,.T.);
#3913=ORIENTED_EDGE('',*,*,#3128,.T.);
#3914=ORIENTED_EDGE('',*,*,#3158,.T.);
#3915=ORIENTED_EDGE('',*,*,#3156,.T.);
#3916=ORIENTED_EDGE('',*,*,#3141,.F.);
#3917=ORIENTED_EDGE('',*,*,#3152,.F.);
#3918=ORIENTED_EDGE('',*,*,#3158,.F.);
#3919=ORIENTED_EDGE('',*,*,#3151,.F.);
#3920=ORIENTED_EDGE('',*,*,#3154,.F.);
#3921=ORIENTED_EDGE('',*,*,#3157,.F.);
#3922=ORIENTED_EDGE('',*,*,#3159,.F.);
#3923=ORIENTED_EDGE('',*,*,#3160,.T.);
#3924=ORIENTED_EDGE('',*,*,#3161,.F.);
#3925=ORIENTED_EDGE('',*,*,#3160,.F.);
#3926=ORIENTED_EDGE('',*,*,#3162,.F.);
#3927=ORIENTED_EDGE('',*,*,#3163,.T.);
#3928=ORIENTED_EDGE('',*,*,#3164,.F.);
#3929=ORIENTED_EDGE('',*,*,#3163,.F.);
#3930=ORIENTED_EDGE('',*,*,#3165,.F.);
#3931=ORIENTED_EDGE('',*,*,#3166,.T.);
#3932=ORIENTED_EDGE('',*,*,#3167,.F.);
#3933=ORIENTED_EDGE('',*,*,#3166,.F.);
#3934=ORIENTED_EDGE('',*,*,#3168,.F.);
#3935=ORIENTED_EDGE('',*,*,#3169,.T.);
#3936=ORIENTED_EDGE('',*,*,#3170,.F.);
#3937=ORIENTED_EDGE('',*,*,#3169,.F.);
#3938=ORIENTED_EDGE('',*,*,#3171,.F.);
#3939=ORIENTED_EDGE('',*,*,#3172,.T.);
#3940=ORIENTED_EDGE('',*,*,#3173,.F.);
#3941=ORIENTED_EDGE('',*,*,#3174,.F.);
#3942=ORIENTED_EDGE('',*,*,#3175,.F.);
#3943=ORIENTED_EDGE('',*,*,#3176,.T.);
#3944=ORIENTED_EDGE('',*,*,#3177,.F.);
#3945=ORIENTED_EDGE('',*,*,#3178,.F.);
#3946=ORIENTED_EDGE('',*,*,#3179,.F.);
#3947=ORIENTED_EDGE('',*,*,#3180,.F.);
#3948=ORIENTED_EDGE('',*,*,#3181,.F.);
#3949=ORIENTED_EDGE('',*,*,#3172,.F.);
#3950=ORIENTED_EDGE('',*,*,#3182,.F.);
#3951=ORIENTED_EDGE('',*,*,#3183,.F.);
#3952=ORIENTED_EDGE('',*,*,#3184,.F.);
#3953=ORIENTED_EDGE('',*,*,#3176,.F.);
#3954=ORIENTED_EDGE('',*,*,#3173,.T.);
#3955=ORIENTED_EDGE('',*,*,#3181,.T.);
#3956=ORIENTED_EDGE('',*,*,#3185,.T.);
#3957=ORIENTED_EDGE('',*,*,#3177,.T.);
#3958=ORIENTED_EDGE('',*,*,#3184,.T.);
#3959=ORIENTED_EDGE('',*,*,#3186,.T.);
#3960=ORIENTED_EDGE('',*,*,#3187,.T.);
#3961=ORIENTED_EDGE('',*,*,#3188,.T.);
#3962=ORIENTED_EDGE('',*,*,#3189,.T.);
#3963=ORIENTED_EDGE('',*,*,#3190,.T.);
#3964=ORIENTED_EDGE('',*,*,#3161,.T.);
#3965=ORIENTED_EDGE('',*,*,#3164,.T.);
#3966=ORIENTED_EDGE('',*,*,#3167,.T.);
#3967=ORIENTED_EDGE('',*,*,#3170,.T.);
#3968=ORIENTED_EDGE('',*,*,#3183,.T.);
#3969=ORIENTED_EDGE('',*,*,#3191,.F.);
#3970=ORIENTED_EDGE('',*,*,#3192,.T.);
#3971=ORIENTED_EDGE('',*,*,#3186,.F.);
#3972=ORIENTED_EDGE('',*,*,#3174,.T.);
#3973=ORIENTED_EDGE('',*,*,#3190,.F.);
#3974=ORIENTED_EDGE('',*,*,#3193,.F.);
#3975=ORIENTED_EDGE('',*,*,#3194,.F.);
#3976=ORIENTED_EDGE('',*,*,#3180,.T.);
#3977=ORIENTED_EDGE('',*,*,#3195,.F.);
#3978=ORIENTED_EDGE('',*,*,#3178,.T.);
#3979=ORIENTED_EDGE('',*,*,#3185,.F.);
#3980=ORIENTED_EDGE('',*,*,#3196,.F.);
#3981=ORIENTED_EDGE('',*,*,#3193,.T.);
#3982=ORIENTED_EDGE('',*,*,#3189,.F.);
#3983=ORIENTED_EDGE('',*,*,#3197,.F.);
#3984=ORIENTED_EDGE('',*,*,#3198,.F.);
#3985=ORIENTED_EDGE('',*,*,#3197,.T.);
#3986=ORIENTED_EDGE('',*,*,#3188,.F.);
#3987=ORIENTED_EDGE('',*,*,#3199,.F.);
#3988=ORIENTED_EDGE('',*,*,#3200,.F.);
#3989=ORIENTED_EDGE('',*,*,#3199,.T.);
#3990=ORIENTED_EDGE('',*,*,#3187,.F.);
#3991=ORIENTED_EDGE('',*,*,#3192,.F.);
#3992=ORIENTED_EDGE('',*,*,#3171,.T.);
#3993=ORIENTED_EDGE('',*,*,#3194,.T.);
#3994=ORIENTED_EDGE('',*,*,#3196,.T.);
#3995=ORIENTED_EDGE('',*,*,#3198,.T.);
#3996=ORIENTED_EDGE('',*,*,#3200,.T.);
#3997=ORIENTED_EDGE('',*,*,#3191,.T.);
#3998=ORIENTED_EDGE('',*,*,#3182,.T.);
#3999=ORIENTED_EDGE('',*,*,#3175,.T.);
#4000=ORIENTED_EDGE('',*,*,#3195,.T.);
#4001=ORIENTED_EDGE('',*,*,#3179,.T.);
#4002=ORIENTED_EDGE('',*,*,#3159,.T.);
#4003=ORIENTED_EDGE('',*,*,#3162,.T.);
#4004=ORIENTED_EDGE('',*,*,#3165,.T.);
#4005=ORIENTED_EDGE('',*,*,#3168,.T.);
#4006=ORIENTED_EDGE('',*,*,#3201,.F.);
#4007=ORIENTED_EDGE('',*,*,#3202,.T.);
#4008=ORIENTED_EDGE('',*,*,#3203,.F.);
#4009=ORIENTED_EDGE('',*,*,#3204,.T.);
#4010=ORIENTED_EDGE('',*,*,#3201,.T.);
#4011=ORIENTED_EDGE('',*,*,#3204,.F.);
#4012=ORIENTED_EDGE('',*,*,#3203,.T.);
#4013=ORIENTED_EDGE('',*,*,#3205,.T.);
#4014=ORIENTED_EDGE('',*,*,#3205,.F.);
#4015=ORIENTED_EDGE('',*,*,#3206,.T.);
#4016=ORIENTED_EDGE('',*,*,#3207,.T.);
#4017=ORIENTED_EDGE('',*,*,#3206,.F.);
#4018=ORIENTED_EDGE('',*,*,#3202,.F.);
#4019=ORIENTED_EDGE('',*,*,#3208,.T.);
#4020=ORIENTED_EDGE('',*,*,#3209,.T.);
#4021=ORIENTED_EDGE('',*,*,#3208,.F.);
#4022=ORIENTED_EDGE('',*,*,#3209,.F.);
#4023=ORIENTED_EDGE('',*,*,#3207,.F.);
#4024=ORIENTED_EDGE('',*,*,#3210,.F.);
#4025=ORIENTED_EDGE('',*,*,#3211,.T.);
#4026=ORIENTED_EDGE('',*,*,#3210,.T.);
#4027=ORIENTED_EDGE('',*,*,#3211,.F.);
#4028=ORIENTED_EDGE('',*,*,#3212,.F.);
#4029=ORIENTED_EDGE('',*,*,#3213,.T.);
#4030=ORIENTED_EDGE('',*,*,#3214,.T.);
#4031=ORIENTED_EDGE('',*,*,#3213,.F.);
#4032=ORIENTED_EDGE('',*,*,#3214,.F.);
#4033=ORIENTED_EDGE('',*,*,#3215,.F.);
#4034=ORIENTED_EDGE('',*,*,#3216,.F.);
#4035=ORIENTED_EDGE('',*,*,#3217,.T.);
#4036=ORIENTED_EDGE('',*,*,#3215,.T.);
#4037=ORIENTED_EDGE('',*,*,#3217,.F.);
#4038=ORIENTED_EDGE('',*,*,#3218,.F.);
#4039=ORIENTED_EDGE('',*,*,#3219,.T.);
#4040=ORIENTED_EDGE('',*,*,#3220,.T.);
#4041=ORIENTED_EDGE('',*,*,#3219,.F.);
#4042=ORIENTED_EDGE('',*,*,#3218,.T.);
#4043=ORIENTED_EDGE('',*,*,#3216,.T.);
#4044=ORIENTED_EDGE('',*,*,#3220,.F.);
#4045=ORIENTED_EDGE('',*,*,#3212,.T.);
#4046=ORIENTED_EDGE('',*,*,#3221,.F.);
#4047=ORIENTED_EDGE('',*,*,#3222,.T.);
#4048=ORIENTED_EDGE('',*,*,#3223,.F.);
#4049=ORIENTED_EDGE('',*,*,#3222,.F.);
#4050=ORIENTED_EDGE('',*,*,#3221,.T.);
#4051=ORIENTED_EDGE('',*,*,#3224,.F.);
#4052=ORIENTED_EDGE('',*,*,#3225,.T.);
#4053=ORIENTED_EDGE('',*,*,#3226,.F.);
#4054=ORIENTED_EDGE('',*,*,#3225,.F.);
#4055=ORIENTED_EDGE('',*,*,#3224,.T.);
#4056=ORIENTED_EDGE('',*,*,#3227,.F.);
#4057=ORIENTED_EDGE('',*,*,#3228,.T.);
#4058=ORIENTED_EDGE('',*,*,#3229,.F.);
#4059=ORIENTED_EDGE('',*,*,#3228,.F.);
#4060=ORIENTED_EDGE('',*,*,#3230,.F.);
#4061=ORIENTED_EDGE('',*,*,#3231,.T.);
#4062=ORIENTED_EDGE('',*,*,#3232,.F.);
#4063=ORIENTED_EDGE('',*,*,#3231,.F.);
#4064=ORIENTED_EDGE('',*,*,#3233,.F.);
#4065=ORIENTED_EDGE('',*,*,#3234,.T.);
#4066=ORIENTED_EDGE('',*,*,#3235,.F.);
#4067=ORIENTED_EDGE('',*,*,#3234,.F.);
#4068=ORIENTED_EDGE('',*,*,#3236,.F.);
#4069=ORIENTED_EDGE('',*,*,#3237,.T.);
#4070=ORIENTED_EDGE('',*,*,#3238,.F.);
#4071=ORIENTED_EDGE('',*,*,#3237,.F.);
#4072=ORIENTED_EDGE('',*,*,#3239,.F.);
#4073=ORIENTED_EDGE('',*,*,#3240,.T.);
#4074=ORIENTED_EDGE('',*,*,#3241,.F.);
#4075=ORIENTED_EDGE('',*,*,#3240,.F.);
#4076=ORIENTED_EDGE('',*,*,#3242,.T.);
#4077=ORIENTED_EDGE('',*,*,#3243,.T.);
#4078=ORIENTED_EDGE('',*,*,#3244,.F.);
#4079=ORIENTED_EDGE('',*,*,#3245,.F.);
#4080=ORIENTED_EDGE('',*,*,#3246,.T.);
#4081=ORIENTED_EDGE('',*,*,#3245,.T.);
#4082=ORIENTED_EDGE('',*,*,#3247,.F.);
#4083=ORIENTED_EDGE('',*,*,#3248,.F.);
#4084=ORIENTED_EDGE('',*,*,#3249,.T.);
#4085=ORIENTED_EDGE('',*,*,#3248,.T.);
#4086=ORIENTED_EDGE('',*,*,#3250,.F.);
#4087=ORIENTED_EDGE('',*,*,#3251,.F.);
#4088=ORIENTED_EDGE('',*,*,#3252,.T.);
#4089=ORIENTED_EDGE('',*,*,#3251,.T.);
#4090=ORIENTED_EDGE('',*,*,#3253,.F.);
#4091=ORIENTED_EDGE('',*,*,#3243,.F.);
#4092=ORIENTED_EDGE('',*,*,#3253,.T.);
#4093=ORIENTED_EDGE('',*,*,#3250,.T.);
#4094=ORIENTED_EDGE('',*,*,#3247,.T.);
#4095=ORIENTED_EDGE('',*,*,#3244,.T.);
#4096=ORIENTED_EDGE('',*,*,#3223,.T.);
#4097=ORIENTED_EDGE('',*,*,#3226,.T.);
#4098=ORIENTED_EDGE('',*,*,#3241,.T.);
#4099=ORIENTED_EDGE('',*,*,#3238,.T.);
#4100=ORIENTED_EDGE('',*,*,#3235,.T.);
#4101=ORIENTED_EDGE('',*,*,#3232,.T.);
#4102=ORIENTED_EDGE('',*,*,#3229,.T.);
#4103=ORIENTED_EDGE('',*,*,#3252,.F.);
#4104=ORIENTED_EDGE('',*,*,#3242,.F.);
#4105=ORIENTED_EDGE('',*,*,#3246,.F.);
#4106=ORIENTED_EDGE('',*,*,#3249,.F.);
#4107=ORIENTED_EDGE('',*,*,#3239,.T.);
#4108=ORIENTED_EDGE('',*,*,#3236,.T.);
#4109=ORIENTED_EDGE('',*,*,#3233,.T.);
#4110=ORIENTED_EDGE('',*,*,#3230,.T.);
#4111=ORIENTED_EDGE('',*,*,#3227,.T.);
#4112=ORIENTED_EDGE('',*,*,#3254,.F.);
#4113=ORIENTED_EDGE('',*,*,#3255,.F.);
#4114=ORIENTED_EDGE('',*,*,#3255,.T.);
#4115=ORIENTED_EDGE('',*,*,#3256,.T.);
#4116=ORIENTED_EDGE('',*,*,#3257,.T.);
#4117=ORIENTED_EDGE('',*,*,#3256,.F.);
#4118=ORIENTED_EDGE('',*,*,#3258,.F.);
#4119=ORIENTED_EDGE('',*,*,#3259,.T.);
#4120=ORIENTED_EDGE('',*,*,#3260,.T.);
#4121=ORIENTED_EDGE('',*,*,#3259,.F.);
#4122=ORIENTED_EDGE('',*,*,#3258,.T.);
#4123=ORIENTED_EDGE('',*,*,#3254,.T.);
#4124=ORIENTED_EDGE('',*,*,#3260,.F.);
#4125=ORIENTED_EDGE('',*,*,#3257,.F.);
#4126=ORIENTED_EDGE('',*,*,#3261,.T.);
#4127=ORIENTED_EDGE('',*,*,#3262,.T.);
#4128=ORIENTED_EDGE('',*,*,#3263,.T.);
#4129=ORIENTED_EDGE('',*,*,#3264,.F.);
#4130=ORIENTED_EDGE('',*,*,#3265,.T.);
#4131=ORIENTED_EDGE('',*,*,#3266,.T.);
#4132=ORIENTED_EDGE('',*,*,#3267,.T.);
#4133=ORIENTED_EDGE('',*,*,#3262,.F.);
#4134=ORIENTED_EDGE('',*,*,#3268,.T.);
#4135=ORIENTED_EDGE('',*,*,#3269,.T.);
#4136=ORIENTED_EDGE('',*,*,#3270,.T.);
#4137=ORIENTED_EDGE('',*,*,#3266,.F.);
#4138=ORIENTED_EDGE('',*,*,#3271,.T.);
#4139=ORIENTED_EDGE('',*,*,#3272,.T.);
#4140=ORIENTED_EDGE('',*,*,#3273,.T.);
#4141=ORIENTED_EDGE('',*,*,#3269,.F.);
#4142=ORIENTED_EDGE('',*,*,#3274,.T.);
#4143=ORIENTED_EDGE('',*,*,#3275,.T.);
#4144=ORIENTED_EDGE('',*,*,#3276,.T.);
#4145=ORIENTED_EDGE('',*,*,#3272,.F.);
#4146=ORIENTED_EDGE('',*,*,#3277,.T.);
#4147=ORIENTED_EDGE('',*,*,#3264,.T.);
#4148=ORIENTED_EDGE('',*,*,#3278,.T.);
#4149=ORIENTED_EDGE('',*,*,#3275,.F.);
#4150=ORIENTED_EDGE('',*,*,#3277,.F.);
#4151=ORIENTED_EDGE('',*,*,#3274,.F.);
#4152=ORIENTED_EDGE('',*,*,#3271,.F.);
#4153=ORIENTED_EDGE('',*,*,#3268,.F.);
#4154=ORIENTED_EDGE('',*,*,#3265,.F.);
#4155=ORIENTED_EDGE('',*,*,#3261,.F.);
#4156=ORIENTED_EDGE('',*,*,#3278,.F.);
#4157=ORIENTED_EDGE('',*,*,#3263,.F.);
#4158=ORIENTED_EDGE('',*,*,#3267,.F.);
#4159=ORIENTED_EDGE('',*,*,#3270,.F.);
#4160=ORIENTED_EDGE('',*,*,#3273,.F.);
#4161=ORIENTED_EDGE('',*,*,#3276,.F.);
#4162=ORIENTED_EDGE('',*,*,#3279,.T.);
#4163=ORIENTED_EDGE('',*,*,#3280,.F.);
#4164=ORIENTED_EDGE('',*,*,#3279,.F.);
#4165=ORIENTED_EDGE('',*,*,#3281,.T.);
#4166=ORIENTED_EDGE('',*,*,#3282,.T.);
#4167=ORIENTED_EDGE('',*,*,#3281,.F.);
#4168=ORIENTED_EDGE('',*,*,#3282,.F.);
#4169=ORIENTED_EDGE('',*,*,#3283,.F.);
#4170=ORIENTED_EDGE('',*,*,#3284,.F.);
#4171=ORIENTED_EDGE('',*,*,#3285,.T.);
#4172=ORIENTED_EDGE('',*,*,#3283,.T.);
#4173=ORIENTED_EDGE('',*,*,#3285,.F.);
#4174=ORIENTED_EDGE('',*,*,#3286,.F.);
#4175=ORIENTED_EDGE('',*,*,#3287,.T.);
#4176=ORIENTED_EDGE('',*,*,#3284,.T.);
#4177=ORIENTED_EDGE('',*,*,#3287,.F.);
#4178=ORIENTED_EDGE('',*,*,#3288,.F.);
#4179=ORIENTED_EDGE('',*,*,#3289,.T.);
#4180=ORIENTED_EDGE('',*,*,#3286,.T.);
#4181=ORIENTED_EDGE('',*,*,#3289,.F.);
#4182=ORIENTED_EDGE('',*,*,#3288,.T.);
#4183=ORIENTED_EDGE('',*,*,#3290,.F.);
#4184=ORIENTED_EDGE('',*,*,#3291,.F.);
#4185=ORIENTED_EDGE('',*,*,#3292,.T.);
#4186=ORIENTED_EDGE('',*,*,#3290,.T.);
#4187=ORIENTED_EDGE('',*,*,#3292,.F.);
#4188=ORIENTED_EDGE('',*,*,#3280,.T.);
#4189=ORIENTED_EDGE('',*,*,#3293,.T.);
#4190=ORIENTED_EDGE('',*,*,#3291,.T.);
#4191=ORIENTED_EDGE('',*,*,#3293,.F.);
#4192=ORIENTED_EDGE('',*,*,#3294,.T.);
#4193=ORIENTED_EDGE('',*,*,#3295,.T.);
#4194=ORIENTED_EDGE('',*,*,#3296,.T.);
#4195=ORIENTED_EDGE('',*,*,#3295,.F.);
#4196=ORIENTED_EDGE('',*,*,#3296,.F.);
#4197=ORIENTED_EDGE('',*,*,#3297,.T.);
#4198=ORIENTED_EDGE('',*,*,#3298,.T.);
#4199=ORIENTED_EDGE('',*,*,#3297,.F.);
#4200=ORIENTED_EDGE('',*,*,#3299,.T.);
#4201=ORIENTED_EDGE('',*,*,#3294,.F.);
#4202=ORIENTED_EDGE('',*,*,#3299,.F.);
#4203=ORIENTED_EDGE('',*,*,#3300,.T.);
#4204=ORIENTED_EDGE('',*,*,#3301,.T.);
#4205=ORIENTED_EDGE('',*,*,#3300,.F.);
#4206=ORIENTED_EDGE('',*,*,#3301,.F.);
#4207=ORIENTED_EDGE('',*,*,#3298,.F.);
#4208=ORIENTED_EDGE('',*,*,#3302,.F.);
#4209=ORIENTED_EDGE('',*,*,#3303,.F.);
#4210=ORIENTED_EDGE('',*,*,#3304,.T.);
#4211=ORIENTED_EDGE('',*,*,#3305,.F.);
#4212=ORIENTED_EDGE('',*,*,#3304,.F.);
#4213=ORIENTED_EDGE('',*,*,#3306,.F.);
#4214=ORIENTED_EDGE('',*,*,#3307,.F.);
#4215=ORIENTED_EDGE('',*,*,#3308,.F.);
#4216=ORIENTED_EDGE('',*,*,#3309,.F.);
#4217=ORIENTED_EDGE('',*,*,#3310,.F.);
#4218=ORIENTED_EDGE('',*,*,#3311,.T.);
#4219=ORIENTED_EDGE('',*,*,#3312,.F.);
#4220=ORIENTED_EDGE('',*,*,#3313,.F.);
#4221=ORIENTED_EDGE('',*,*,#3314,.F.);
#4222=ORIENTED_EDGE('',*,*,#3315,.F.);
#4223=ORIENTED_EDGE('',*,*,#3316,.F.);
#4224=ORIENTED_EDGE('',*,*,#3317,.F.);
#4225=ORIENTED_EDGE('',*,*,#3311,.F.);
#4226=ORIENTED_EDGE('',*,*,#3307,.T.);
#4227=ORIENTED_EDGE('',*,*,#3318,.T.);
#4228=ORIENTED_EDGE('',*,*,#3316,.T.);
#4229=ORIENTED_EDGE('',*,*,#3319,.F.);
#4230=ORIENTED_EDGE('',*,*,#3306,.T.);
#4231=ORIENTED_EDGE('',*,*,#3320,.T.);
#4232=ORIENTED_EDGE('',*,*,#3317,.T.);
#4233=ORIENTED_EDGE('',*,*,#3318,.F.);
#4234=ORIENTED_EDGE('',*,*,#3303,.T.);
#4235=ORIENTED_EDGE('',*,*,#3321,.T.);
#4236=ORIENTED_EDGE('',*,*,#3312,.T.);
#4237=ORIENTED_EDGE('',*,*,#3320,.F.);
#4238=ORIENTED_EDGE('',*,*,#3322,.F.);
#4239=ORIENTED_EDGE('',*,*,#3323,.T.);
#4240=ORIENTED_EDGE('',*,*,#3324,.T.);
#4241=ORIENTED_EDGE('',*,*,#3323,.F.);
#4242=ORIENTED_EDGE('',*,*,#3302,.T.);
#4243=ORIENTED_EDGE('',*,*,#3325,.T.);
#4244=ORIENTED_EDGE('',*,*,#3313,.T.);
#4245=ORIENTED_EDGE('',*,*,#3321,.F.);
#4246=ORIENTED_EDGE('',*,*,#3308,.T.);
#4247=ORIENTED_EDGE('',*,*,#3319,.T.);
#4248=ORIENTED_EDGE('',*,*,#3315,.T.);
#4249=ORIENTED_EDGE('',*,*,#3326,.F.);
#4250=ORIENTED_EDGE('',*,*,#3309,.T.);
#4251=ORIENTED_EDGE('',*,*,#3326,.T.);
#4252=ORIENTED_EDGE('',*,*,#3314,.T.);
#4253=ORIENTED_EDGE('',*,*,#3325,.F.);
#4254=ORIENTED_EDGE('',*,*,#3310,.T.);
#4255=ORIENTED_EDGE('',*,*,#3322,.T.);
#4256=ORIENTED_EDGE('',*,*,#3305,.T.);
#4257=ORIENTED_EDGE('',*,*,#3324,.F.);
#4258=ORIENTED_EDGE('',*,*,#3327,.F.);
#4259=ORIENTED_EDGE('',*,*,#3328,.T.);
#4260=ORIENTED_EDGE('',*,*,#3329,.T.);
#4261=ORIENTED_EDGE('',*,*,#3328,.F.);
#4262=ORIENTED_EDGE('',*,*,#3330,.F.);
#4263=ORIENTED_EDGE('',*,*,#3331,.T.);
#4264=ORIENTED_EDGE('',*,*,#3332,.T.);
#4265=ORIENTED_EDGE('',*,*,#3331,.F.);
#4266=ORIENTED_EDGE('',*,*,#3330,.T.);
#4267=ORIENTED_EDGE('',*,*,#3327,.T.);
#4268=ORIENTED_EDGE('',*,*,#3332,.F.);
#4269=ORIENTED_EDGE('',*,*,#3329,.F.);
#4270=ORIENTED_EDGE('',*,*,#3333,.F.);
#4271=ORIENTED_EDGE('',*,*,#3334,.F.);
#4272=ORIENTED_EDGE('',*,*,#3335,.T.);
#4273=ORIENTED_EDGE('',*,*,#3333,.T.);
#4274=ORIENTED_EDGE('',*,*,#3335,.F.);
#4275=ORIENTED_EDGE('',*,*,#3336,.F.);
#4276=ORIENTED_EDGE('',*,*,#3337,.T.);
#4277=ORIENTED_EDGE('',*,*,#3334,.T.);
#4278=ORIENTED_EDGE('',*,*,#3337,.F.);
#4279=ORIENTED_EDGE('',*,*,#3338,.F.);
#4280=ORIENTED_EDGE('',*,*,#3339,.T.);
#4281=ORIENTED_EDGE('',*,*,#3336,.T.);
#4282=ORIENTED_EDGE('',*,*,#3339,.F.);
#4283=ORIENTED_EDGE('',*,*,#3338,.T.);
#4284=ORIENTED_EDGE('',*,*,#3340,.F.);
#4285=ORIENTED_EDGE('',*,*,#3341,.F.);
#4286=ORIENTED_EDGE('',*,*,#3342,.T.);
#4287=ORIENTED_EDGE('',*,*,#3340,.T.);
#4288=ORIENTED_EDGE('',*,*,#3342,.F.);
#4289=ORIENTED_EDGE('',*,*,#3343,.F.);
#4290=ORIENTED_EDGE('',*,*,#3344,.T.);
#4291=ORIENTED_EDGE('',*,*,#3341,.T.);
#4292=ORIENTED_EDGE('',*,*,#3344,.F.);
#4293=ORIENTED_EDGE('',*,*,#3345,.F.);
#4294=ORIENTED_EDGE('',*,*,#3346,.T.);
#4295=ORIENTED_EDGE('',*,*,#3343,.T.);
#4296=ORIENTED_EDGE('',*,*,#3346,.F.);
#4297=ORIENTED_EDGE('',*,*,#3345,.T.);
#4298=ORIENTED_EDGE('',*,*,#3347,.T.);
#4299=ORIENTED_EDGE('',*,*,#3348,.T.);
#4300=ORIENTED_EDGE('',*,*,#3349,.T.);
#4301=ORIENTED_EDGE('',*,*,#3350,.F.);
#4302=ORIENTED_EDGE('',*,*,#3351,.T.);
#4303=ORIENTED_EDGE('',*,*,#3352,.T.);
#4304=ORIENTED_EDGE('',*,*,#3353,.T.);
#4305=ORIENTED_EDGE('',*,*,#3348,.F.);
#4306=ORIENTED_EDGE('',*,*,#3354,.T.);
#4307=ORIENTED_EDGE('',*,*,#3355,.T.);
#4308=ORIENTED_EDGE('',*,*,#3356,.T.);
#4309=ORIENTED_EDGE('',*,*,#3352,.F.);
#4310=ORIENTED_EDGE('',*,*,#3357,.T.);
#4311=ORIENTED_EDGE('',*,*,#3358,.T.);
#4312=ORIENTED_EDGE('',*,*,#3359,.T.);
#4313=ORIENTED_EDGE('',*,*,#3355,.F.);
#4314=ORIENTED_EDGE('',*,*,#3360,.T.);
#4315=ORIENTED_EDGE('',*,*,#3361,.T.);
#4316=ORIENTED_EDGE('',*,*,#3362,.T.);
#4317=ORIENTED_EDGE('',*,*,#3358,.F.);
#4318=ORIENTED_EDGE('',*,*,#3363,.T.);
#4319=ORIENTED_EDGE('',*,*,#3350,.T.);
#4320=ORIENTED_EDGE('',*,*,#3364,.T.);
#4321=ORIENTED_EDGE('',*,*,#3361,.F.);
#4322=ORIENTED_EDGE('',*,*,#3363,.F.);
#4323=ORIENTED_EDGE('',*,*,#3360,.F.);
#4324=ORIENTED_EDGE('',*,*,#3357,.F.);
#4325=ORIENTED_EDGE('',*,*,#3354,.F.);
#4326=ORIENTED_EDGE('',*,*,#3351,.F.);
#4327=ORIENTED_EDGE('',*,*,#3347,.F.);
#4328=ORIENTED_EDGE('',*,*,#3364,.F.);
#4329=ORIENTED_EDGE('',*,*,#3349,.F.);
#4330=ORIENTED_EDGE('',*,*,#3353,.F.);
#4331=ORIENTED_EDGE('',*,*,#3356,.F.);
#4332=ORIENTED_EDGE('',*,*,#3359,.F.);
#4333=ORIENTED_EDGE('',*,*,#3362,.F.);
#4334=ORIENTED_EDGE('',*,*,#3365,.F.);
#4335=ORIENTED_EDGE('',*,*,#3366,.T.);
#4336=ORIENTED_EDGE('',*,*,#3367,.T.);
#4337=ORIENTED_EDGE('',*,*,#3366,.F.);
#4338=ORIENTED_EDGE('',*,*,#3365,.T.);
#4339=ORIENTED_EDGE('',*,*,#3367,.F.);
#4340=ORIENTED_EDGE('',*,*,#3368,.F.);
#4341=ORIENTED_EDGE('',*,*,#3369,.T.);
#4342=ORIENTED_EDGE('',*,*,#3370,.T.);
#4343=ORIENTED_EDGE('',*,*,#3369,.F.);
#4344=ORIENTED_EDGE('',*,*,#3371,.F.);
#4345=ORIENTED_EDGE('',*,*,#3372,.T.);
#4346=ORIENTED_EDGE('',*,*,#3373,.T.);
#4347=ORIENTED_EDGE('',*,*,#3372,.F.);
#4348=ORIENTED_EDGE('',*,*,#3371,.T.);
#4349=ORIENTED_EDGE('',*,*,#3368,.T.);
#4350=ORIENTED_EDGE('',*,*,#3373,.F.);
#4351=ORIENTED_EDGE('',*,*,#3370,.F.);
#4352=ORIENTED_EDGE('',*,*,#3374,.F.);
#4353=ORIENTED_EDGE('',*,*,#3375,.F.);
#4354=ORIENTED_EDGE('',*,*,#3376,.F.);
#4355=ORIENTED_EDGE('',*,*,#3377,.F.);
#4356=ORIENTED_EDGE('',*,*,#3378,.F.);
#4357=ORIENTED_EDGE('',*,*,#3379,.T.);
#4358=ORIENTED_EDGE('',*,*,#3380,.F.);
#4359=ORIENTED_EDGE('',*,*,#3375,.T.);
#4360=ORIENTED_EDGE('',*,*,#3381,.F.);
#4361=ORIENTED_EDGE('',*,*,#3382,.T.);
#4362=ORIENTED_EDGE('',*,*,#3383,.F.);
#4363=ORIENTED_EDGE('',*,*,#3379,.F.);
#4364=ORIENTED_EDGE('',*,*,#3384,.F.);
#4365=ORIENTED_EDGE('',*,*,#3385,.F.);
#4366=ORIENTED_EDGE('',*,*,#3386,.F.);
#4367=ORIENTED_EDGE('',*,*,#3382,.F.);
#4368=ORIENTED_EDGE('',*,*,#3381,.T.);
#4369=ORIENTED_EDGE('',*,*,#3387,.F.);
#4370=ORIENTED_EDGE('',*,*,#3388,.T.);
#4371=ORIENTED_EDGE('',*,*,#3389,.F.);
#4372=ORIENTED_EDGE('',*,*,#3388,.F.);
#4373=ORIENTED_EDGE('',*,*,#3390,.F.);
#4374=ORIENTED_EDGE('',*,*,#3377,.T.);
#4375=ORIENTED_EDGE('',*,*,#3391,.F.);
#4376=ORIENTED_EDGE('',*,*,#3392,.F.);
#4377=ORIENTED_EDGE('',*,*,#3384,.T.);
#4378=ORIENTED_EDGE('',*,*,#3390,.T.);
#4379=ORIENTED_EDGE('',*,*,#3387,.T.);
#4380=ORIENTED_EDGE('',*,*,#3374,.T.);
#4381=ORIENTED_EDGE('',*,*,#3393,.F.);
#4382=ORIENTED_EDGE('',*,*,#3385,.T.);
#4383=ORIENTED_EDGE('',*,*,#3394,.F.);
#4384=ORIENTED_EDGE('',*,*,#3395,.F.);
#4385=ORIENTED_EDGE('',*,*,#3386,.T.);
#4386=ORIENTED_EDGE('',*,*,#3396,.F.);
#4387=ORIENTED_EDGE('',*,*,#3376,.T.);
#4388=ORIENTED_EDGE('',*,*,#3397,.F.);
#4389=ORIENTED_EDGE('',*,*,#3398,.F.);
#4390=ORIENTED_EDGE('',*,*,#3399,.F.);
#4391=ORIENTED_EDGE('',*,*,#3400,.T.);
#4392=ORIENTED_EDGE('',*,*,#3397,.T.);
#4393=ORIENTED_EDGE('',*,*,#3380,.T.);
#4394=ORIENTED_EDGE('',*,*,#3383,.T.);
#4395=ORIENTED_EDGE('',*,*,#3398,.T.);
#4396=ORIENTED_EDGE('',*,*,#3400,.F.);
#4397=ORIENTED_EDGE('',*,*,#3393,.T.);
#4398=ORIENTED_EDGE('',*,*,#3392,.T.);
#4399=ORIENTED_EDGE('',*,*,#3401,.T.);
#4400=ORIENTED_EDGE('',*,*,#3402,.T.);
#4401=ORIENTED_EDGE('',*,*,#3403,.T.);
#4402=ORIENTED_EDGE('',*,*,#3391,.T.);
#4403=ORIENTED_EDGE('',*,*,#3396,.T.);
#4404=ORIENTED_EDGE('',*,*,#3395,.T.);
#4405=ORIENTED_EDGE('',*,*,#3404,.T.);
#4406=ORIENTED_EDGE('',*,*,#3405,.T.);
#4407=ORIENTED_EDGE('',*,*,#3406,.T.);
#4408=ORIENTED_EDGE('',*,*,#3394,.T.);
#4409=ORIENTED_EDGE('',*,*,#3405,.F.);
#4410=ORIENTED_EDGE('',*,*,#3407,.F.);
#4411=ORIENTED_EDGE('',*,*,#3403,.F.);
#4412=ORIENTED_EDGE('',*,*,#3408,.T.);
#4413=ORIENTED_EDGE('',*,*,#3401,.F.);
#4414=ORIENTED_EDGE('',*,*,#3406,.F.);
#4415=ORIENTED_EDGE('',*,*,#3407,.T.);
#4416=ORIENTED_EDGE('',*,*,#3404,.F.);
#4417=ORIENTED_EDGE('',*,*,#3402,.F.);
#4418=ORIENTED_EDGE('',*,*,#3408,.F.);
#4419=ORIENTED_EDGE('',*,*,#3409,.F.);
#4420=ORIENTED_EDGE('',*,*,#3410,.F.);
#4421=ORIENTED_EDGE('',*,*,#3411,.T.);
#4422=ORIENTED_EDGE('',*,*,#3412,.T.);
#4423=ORIENTED_EDGE('',*,*,#3411,.F.);
#4424=ORIENTED_EDGE('',*,*,#3413,.F.);
#4425=ORIENTED_EDGE('',*,*,#3412,.F.);
#4426=ORIENTED_EDGE('',*,*,#3378,.T.);
#4427=ORIENTED_EDGE('',*,*,#3414,.F.);
#4428=ORIENTED_EDGE('',*,*,#3415,.T.);
#4429=ORIENTED_EDGE('',*,*,#3409,.T.);
#4430=ORIENTED_EDGE('',*,*,#3413,.T.);
#4431=ORIENTED_EDGE('',*,*,#3410,.T.);
#4432=ORIENTED_EDGE('',*,*,#3416,.T.);
#4433=ORIENTED_EDGE('',*,*,#3417,.T.);
#4434=ORIENTED_EDGE('',*,*,#3416,.F.);
#4435=ORIENTED_EDGE('',*,*,#3415,.F.);
#4436=ORIENTED_EDGE('',*,*,#3414,.T.);
#4437=ORIENTED_EDGE('',*,*,#3389,.T.);
#4438=ORIENTED_EDGE('',*,*,#3417,.F.);
#4439=ORIENTED_EDGE('',*,*,#3399,.T.);
#4440=ORIENTED_EDGE('',*,*,#3418,.F.);
#4441=ORIENTED_EDGE('',*,*,#3419,.T.);
#4442=ORIENTED_EDGE('',*,*,#3420,.T.);
#4443=ORIENTED_EDGE('',*,*,#3419,.F.);
#4444=ORIENTED_EDGE('',*,*,#3421,.F.);
#4445=ORIENTED_EDGE('',*,*,#3422,.T.);
#4446=ORIENTED_EDGE('',*,*,#3423,.T.);
#4447=ORIENTED_EDGE('',*,*,#3422,.F.);
#4448=ORIENTED_EDGE('',*,*,#3421,.T.);
#4449=ORIENTED_EDGE('',*,*,#3418,.T.);
#4450=ORIENTED_EDGE('',*,*,#3423,.F.);
#4451=ORIENTED_EDGE('',*,*,#3420,.F.);
#4452=ORIENTED_EDGE('',*,*,#3424,.F.);
#4453=ORIENTED_EDGE('',*,*,#3425,.T.);
#4454=ORIENTED_EDGE('',*,*,#3426,.T.);
#4455=ORIENTED_EDGE('',*,*,#3425,.F.);
#4456=ORIENTED_EDGE('',*,*,#3427,.F.);
#4457=ORIENTED_EDGE('',*,*,#3428,.T.);
#4458=ORIENTED_EDGE('',*,*,#3429,.T.);
#4459=ORIENTED_EDGE('',*,*,#3428,.F.);
#4460=ORIENTED_EDGE('',*,*,#3427,.T.);
#4461=ORIENTED_EDGE('',*,*,#3424,.T.);
#4462=ORIENTED_EDGE('',*,*,#3429,.F.);
#4463=ORIENTED_EDGE('',*,*,#3426,.F.);
#4464=ORIENTED_EDGE('',*,*,#3430,.F.);
#4465=ORIENTED_EDGE('',*,*,#3431,.T.);
#4466=ORIENTED_EDGE('',*,*,#3432,.T.);
#4467=ORIENTED_EDGE('',*,*,#3431,.F.);
#4468=ORIENTED_EDGE('',*,*,#3433,.F.);
#4469=ORIENTED_EDGE('',*,*,#3434,.T.);
#4470=ORIENTED_EDGE('',*,*,#3435,.T.);
#4471=ORIENTED_EDGE('',*,*,#3434,.F.);
#4472=ORIENTED_EDGE('',*,*,#3433,.T.);
#4473=ORIENTED_EDGE('',*,*,#3430,.T.);
#4474=ORIENTED_EDGE('',*,*,#3435,.F.);
#4475=ORIENTED_EDGE('',*,*,#3432,.F.);
#4476=ORIENTED_EDGE('',*,*,#3436,.F.);
#4477=ORIENTED_EDGE('',*,*,#3437,.F.);
#4478=ORIENTED_EDGE('',*,*,#3438,.T.);
#4479=ORIENTED_EDGE('',*,*,#3439,.F.);
#4480=ORIENTED_EDGE('',*,*,#3438,.F.);
#4481=ORIENTED_EDGE('',*,*,#3440,.F.);
#4482=ORIENTED_EDGE('',*,*,#3441,.T.);
#4483=ORIENTED_EDGE('',*,*,#3441,.F.);
#4484=ORIENTED_EDGE('',*,*,#3440,.T.);
#4485=ORIENTED_EDGE('',*,*,#3437,.T.);
#4486=ORIENTED_EDGE('',*,*,#3442,.T.);
#4487=ORIENTED_EDGE('',*,*,#3443,.T.);
#4488=ORIENTED_EDGE('',*,*,#3436,.T.);
#4489=ORIENTED_EDGE('',*,*,#3443,.F.);
#4490=ORIENTED_EDGE('',*,*,#3444,.T.);
#4491=ORIENTED_EDGE('',*,*,#3445,.F.);
#4492=ORIENTED_EDGE('',*,*,#3444,.F.);
#4493=ORIENTED_EDGE('',*,*,#3442,.F.);
#4494=ORIENTED_EDGE('',*,*,#3446,.F.);
#4495=ORIENTED_EDGE('',*,*,#3439,.T.);
#4496=ORIENTED_EDGE('',*,*,#3447,.F.);
#4497=ORIENTED_EDGE('',*,*,#3448,.T.);
#4498=ORIENTED_EDGE('',*,*,#3446,.T.);
#4499=ORIENTED_EDGE('',*,*,#3448,.F.);
#4500=ORIENTED_EDGE('',*,*,#3449,.F.);
#4501=ORIENTED_EDGE('',*,*,#3450,.T.);
#4502=ORIENTED_EDGE('',*,*,#3451,.F.);
#4503=ORIENTED_EDGE('',*,*,#3450,.F.);
#4504=ORIENTED_EDGE('',*,*,#3449,.T.);
#4505=ORIENTED_EDGE('',*,*,#3445,.T.);
#4506=ORIENTED_EDGE('',*,*,#3452,.T.);
#4507=ORIENTED_EDGE('',*,*,#3453,.T.);
#4508=ORIENTED_EDGE('',*,*,#3454,.F.);
#4509=ORIENTED_EDGE('',*,*,#3455,.F.);
#4510=ORIENTED_EDGE('',*,*,#3456,.F.);
#4511=ORIENTED_EDGE('',*,*,#3453,.F.);
#4512=ORIENTED_EDGE('',*,*,#3457,.T.);
#4513=ORIENTED_EDGE('',*,*,#3458,.T.);
#4514=ORIENTED_EDGE('',*,*,#3457,.F.);
#4515=ORIENTED_EDGE('',*,*,#3452,.F.);
#4516=ORIENTED_EDGE('',*,*,#3459,.F.);
#4517=ORIENTED_EDGE('',*,*,#3447,.T.);
#4518=ORIENTED_EDGE('',*,*,#3460,.F.);
#4519=ORIENTED_EDGE('',*,*,#3461,.T.);
#4520=ORIENTED_EDGE('',*,*,#3459,.T.);
#4521=ORIENTED_EDGE('',*,*,#3461,.F.);
#4522=ORIENTED_EDGE('',*,*,#3460,.T.);
#4523=ORIENTED_EDGE('',*,*,#3458,.F.);
#4524=ORIENTED_EDGE('',*,*,#3462,.F.);
#4525=ORIENTED_EDGE('',*,*,#3463,.T.);
#4526=ORIENTED_EDGE('',*,*,#3464,.F.);
#4527=ORIENTED_EDGE('',*,*,#3465,.T.);
#4528=ORIENTED_EDGE('',*,*,#3462,.T.);
#4529=ORIENTED_EDGE('',*,*,#3465,.F.);
#4530=ORIENTED_EDGE('',*,*,#3464,.T.);
#4531=ORIENTED_EDGE('',*,*,#3451,.T.);
#4532=ORIENTED_EDGE('',*,*,#3463,.F.);
#4533=ORIENTED_EDGE('',*,*,#3466,.T.);
#4534=ORIENTED_EDGE('',*,*,#3454,.T.);
#4535=ORIENTED_EDGE('',*,*,#3456,.T.);
#4536=ORIENTED_EDGE('',*,*,#3455,.T.);
#4537=ORIENTED_EDGE('',*,*,#3466,.F.);
#4538=ORIENTED_EDGE('',*,*,#3467,.T.);
#4539=ORIENTED_EDGE('',*,*,#3468,.T.);
#4540=ORIENTED_EDGE('',*,*,#3469,.T.);
#4541=ORIENTED_EDGE('',*,*,#3470,.T.);
#4542=ORIENTED_EDGE('',*,*,#3471,.T.);
#4543=ORIENTED_EDGE('',*,*,#3472,.T.);
#4544=ORIENTED_EDGE('',*,*,#3473,.F.);
#4545=ORIENTED_EDGE('',*,*,#3474,.T.);
#4546=ORIENTED_EDGE('',*,*,#3475,.T.);
#4547=ORIENTED_EDGE('',*,*,#3476,.T.);
#4548=ORIENTED_EDGE('',*,*,#3477,.T.);
#4549=ORIENTED_EDGE('',*,*,#3478,.T.);
#4550=ORIENTED_EDGE('',*,*,#3479,.T.);
#4551=ORIENTED_EDGE('',*,*,#3480,.F.);
#4552=ORIENTED_EDGE('',*,*,#3481,.F.);
#4553=ORIENTED_EDGE('',*,*,#3479,.F.);
#4554=ORIENTED_EDGE('',*,*,#3482,.F.);
#4555=ORIENTED_EDGE('',*,*,#3468,.F.);
#4556=ORIENTED_EDGE('',*,*,#3482,.T.);
#4557=ORIENTED_EDGE('',*,*,#3478,.F.);
#4558=ORIENTED_EDGE('',*,*,#3483,.F.);
#4559=ORIENTED_EDGE('',*,*,#3469,.F.);
#4560=ORIENTED_EDGE('',*,*,#3483,.T.);
#4561=ORIENTED_EDGE('',*,*,#3477,.F.);
#4562=ORIENTED_EDGE('',*,*,#3484,.F.);
#4563=ORIENTED_EDGE('',*,*,#3470,.F.);
#4564=ORIENTED_EDGE('',*,*,#3484,.T.);
#4565=ORIENTED_EDGE('',*,*,#3476,.F.);
#4566=ORIENTED_EDGE('',*,*,#3485,.F.);
#4567=ORIENTED_EDGE('',*,*,#3471,.F.);
#4568=ORIENTED_EDGE('',*,*,#3485,.T.);
#4569=ORIENTED_EDGE('',*,*,#3475,.F.);
#4570=ORIENTED_EDGE('',*,*,#3486,.F.);
#4571=ORIENTED_EDGE('',*,*,#3472,.F.);
#4572=ORIENTED_EDGE('',*,*,#3486,.T.);
#4573=ORIENTED_EDGE('',*,*,#3474,.F.);
#4574=ORIENTED_EDGE('',*,*,#3481,.T.);
#4575=ORIENTED_EDGE('',*,*,#3467,.F.);
#4576=ORIENTED_EDGE('',*,*,#3480,.T.);
#4577=ORIENTED_EDGE('',*,*,#3487,.T.);
#4578=ORIENTED_EDGE('',*,*,#3488,.T.);
#4579=ORIENTED_EDGE('',*,*,#3487,.F.);
#4580=ORIENTED_EDGE('',*,*,#3489,.F.);
#4581=ORIENTED_EDGE('',*,*,#3490,.T.);
#4582=ORIENTED_EDGE('',*,*,#3488,.F.);
#4583=ORIENTED_EDGE('',*,*,#3491,.T.);
#4584=ORIENTED_EDGE('',*,*,#3489,.T.);
#4585=ORIENTED_EDGE('',*,*,#3491,.F.);
#4586=ORIENTED_EDGE('',*,*,#3492,.F.);
#4587=ORIENTED_EDGE('',*,*,#3493,.T.);
#4588=ORIENTED_EDGE('',*,*,#3473,.T.);
#4589=ORIENTED_EDGE('',*,*,#3493,.F.);
#4590=ORIENTED_EDGE('',*,*,#3494,.F.);
#4591=ORIENTED_EDGE('',*,*,#3495,.T.);
#4592=ORIENTED_EDGE('',*,*,#3492,.T.);
#4593=ORIENTED_EDGE('',*,*,#3495,.F.);
#4594=ORIENTED_EDGE('',*,*,#3494,.T.);
#4595=ORIENTED_EDGE('',*,*,#3496,.F.);
#4596=ORIENTED_EDGE('',*,*,#3496,.T.);
#4597=ORIENTED_EDGE('',*,*,#3497,.T.);
#4598=ORIENTED_EDGE('',*,*,#3490,.F.);
#4599=ORIENTED_EDGE('',*,*,#3497,.F.);
#4600=ORIENTED_EDGE('',*,*,#3498,.F.);
#4601=ORIENTED_EDGE('',*,*,#3499,.T.);
#4602=ORIENTED_EDGE('',*,*,#3500,.F.);
#4603=ORIENTED_EDGE('',*,*,#3499,.F.);
#4604=ORIENTED_EDGE('',*,*,#3501,.F.);
#4605=ORIENTED_EDGE('',*,*,#3502,.T.);
#4606=ORIENTED_EDGE('',*,*,#3503,.F.);
#4607=ORIENTED_EDGE('',*,*,#3502,.F.);
#4608=ORIENTED_EDGE('',*,*,#3504,.F.);
#4609=ORIENTED_EDGE('',*,*,#3505,.T.);
#4610=ORIENTED_EDGE('',*,*,#3506,.F.);
#4611=ORIENTED_EDGE('',*,*,#3505,.F.);
#4612=ORIENTED_EDGE('',*,*,#3507,.F.);
#4613=ORIENTED_EDGE('',*,*,#3508,.T.);
#4614=ORIENTED_EDGE('',*,*,#3509,.F.);
#4615=ORIENTED_EDGE('',*,*,#3508,.F.);
#4616=ORIENTED_EDGE('',*,*,#3510,.F.);
#4617=ORIENTED_EDGE('',*,*,#3511,.F.);
#4618=ORIENTED_EDGE('',*,*,#3507,.T.);
#4619=ORIENTED_EDGE('',*,*,#3504,.T.);
#4620=ORIENTED_EDGE('',*,*,#3501,.T.);
#4621=ORIENTED_EDGE('',*,*,#3498,.T.);
#4622=ORIENTED_EDGE('',*,*,#3512,.F.);
#4623=ORIENTED_EDGE('',*,*,#3513,.T.);
#4624=ORIENTED_EDGE('',*,*,#3510,.T.);
#4625=ORIENTED_EDGE('',*,*,#3513,.F.);
#4626=ORIENTED_EDGE('',*,*,#3514,.F.);
#4627=ORIENTED_EDGE('',*,*,#3515,.T.);
#4628=ORIENTED_EDGE('',*,*,#3516,.T.);
#4629=ORIENTED_EDGE('',*,*,#3515,.F.);
#4630=ORIENTED_EDGE('',*,*,#3511,.T.);
#4631=ORIENTED_EDGE('',*,*,#3517,.T.);
#4632=ORIENTED_EDGE('',*,*,#3518,.T.);
#4633=ORIENTED_EDGE('',*,*,#3517,.F.);
#4634=ORIENTED_EDGE('',*,*,#3512,.T.);
#4635=ORIENTED_EDGE('',*,*,#3514,.T.);
#4636=ORIENTED_EDGE('',*,*,#3509,.T.);
#4637=ORIENTED_EDGE('',*,*,#3506,.T.);
#4638=ORIENTED_EDGE('',*,*,#3503,.T.);
#4639=ORIENTED_EDGE('',*,*,#3500,.T.);
#4640=ORIENTED_EDGE('',*,*,#3518,.F.);
#4641=ORIENTED_EDGE('',*,*,#3516,.F.);
#4642=ORIENTED_EDGE('',*,*,#3519,.F.);
#4643=ORIENTED_EDGE('',*,*,#3520,.T.);
#4644=ORIENTED_EDGE('',*,*,#3521,.F.);
#4645=ORIENTED_EDGE('',*,*,#3520,.F.);
#4646=ORIENTED_EDGE('',*,*,#3522,.F.);
#4647=ORIENTED_EDGE('',*,*,#3523,.T.);
#4648=ORIENTED_EDGE('',*,*,#3524,.F.);
#4649=ORIENTED_EDGE('',*,*,#3523,.F.);
#4650=ORIENTED_EDGE('',*,*,#3525,.F.);
#4651=ORIENTED_EDGE('',*,*,#3526,.T.);
#4652=ORIENTED_EDGE('',*,*,#3527,.F.);
#4653=ORIENTED_EDGE('',*,*,#3526,.F.);
#4654=ORIENTED_EDGE('',*,*,#3528,.F.);
#4655=ORIENTED_EDGE('',*,*,#3529,.T.);
#4656=ORIENTED_EDGE('',*,*,#3530,.F.);
#4657=ORIENTED_EDGE('',*,*,#3529,.F.);
#4658=ORIENTED_EDGE('',*,*,#3531,.T.);
#4659=ORIENTED_EDGE('',*,*,#3532,.F.);
#4660=ORIENTED_EDGE('',*,*,#3530,.T.);
#4661=ORIENTED_EDGE('',*,*,#3527,.T.);
#4662=ORIENTED_EDGE('',*,*,#3524,.T.);
#4663=ORIENTED_EDGE('',*,*,#3521,.T.);
#4664=ORIENTED_EDGE('',*,*,#3531,.F.);
#4665=ORIENTED_EDGE('',*,*,#3533,.T.);
#4666=ORIENTED_EDGE('',*,*,#3534,.T.);
#4667=ORIENTED_EDGE('',*,*,#3533,.F.);
#4668=ORIENTED_EDGE('',*,*,#3535,.F.);
#4669=ORIENTED_EDGE('',*,*,#3536,.T.);
#4670=ORIENTED_EDGE('',*,*,#3537,.T.);
#4671=ORIENTED_EDGE('',*,*,#3536,.F.);
#4672=ORIENTED_EDGE('',*,*,#3538,.F.);
#4673=ORIENTED_EDGE('',*,*,#3539,.T.);
#4674=ORIENTED_EDGE('',*,*,#3532,.T.);
#4675=ORIENTED_EDGE('',*,*,#3539,.F.);
#4676=ORIENTED_EDGE('',*,*,#3538,.T.);
#4677=ORIENTED_EDGE('',*,*,#3535,.T.);
#4678=ORIENTED_EDGE('',*,*,#3534,.F.);
#4679=ORIENTED_EDGE('',*,*,#3537,.F.);
#4680=ORIENTED_EDGE('',*,*,#3528,.T.);
#4681=ORIENTED_EDGE('',*,*,#3525,.T.);
#4682=ORIENTED_EDGE('',*,*,#3522,.T.);
#4683=ORIENTED_EDGE('',*,*,#3519,.T.);
#4684=ORIENTED_EDGE('',*,*,#3540,.F.);
#4685=ORIENTED_EDGE('',*,*,#3541,.F.);
#4686=ORIENTED_EDGE('',*,*,#3542,.T.);
#4687=ORIENTED_EDGE('',*,*,#3540,.T.);
#4688=ORIENTED_EDGE('',*,*,#3542,.F.);
#4689=ORIENTED_EDGE('',*,*,#3543,.F.);
#4690=ORIENTED_EDGE('',*,*,#3544,.T.);
#4691=ORIENTED_EDGE('',*,*,#3541,.T.);
#4692=ORIENTED_EDGE('',*,*,#3544,.F.);
#4693=ORIENTED_EDGE('',*,*,#3545,.F.);
#4694=ORIENTED_EDGE('',*,*,#3546,.T.);
#4695=ORIENTED_EDGE('',*,*,#3543,.T.);
#4696=ORIENTED_EDGE('',*,*,#3546,.F.);
#4697=ORIENTED_EDGE('',*,*,#3545,.T.);
#4698=ORIENTED_EDGE('',*,*,#3547,.F.);
#4699=ORIENTED_EDGE('',*,*,#3548,.F.);
#4700=ORIENTED_EDGE('',*,*,#3549,.T.);
#4701=ORIENTED_EDGE('',*,*,#3547,.T.);
#4702=ORIENTED_EDGE('',*,*,#3549,.F.);
#4703=ORIENTED_EDGE('',*,*,#3550,.F.);
#4704=ORIENTED_EDGE('',*,*,#3551,.T.);
#4705=ORIENTED_EDGE('',*,*,#3548,.T.);
#4706=ORIENTED_EDGE('',*,*,#3551,.F.);
#4707=ORIENTED_EDGE('',*,*,#3552,.F.);
#4708=ORIENTED_EDGE('',*,*,#3553,.T.);
#4709=ORIENTED_EDGE('',*,*,#3550,.T.);
#4710=ORIENTED_EDGE('',*,*,#3553,.F.);
#4711=ORIENTED_EDGE('',*,*,#3552,.T.);
#4712=ORIENTED_EDGE('',*,*,#3554,.T.);
#4713=ORIENTED_EDGE('',*,*,#3555,.T.);
#4714=ORIENTED_EDGE('',*,*,#3556,.T.);
#4715=ORIENTED_EDGE('',*,*,#3557,.F.);
#4716=ORIENTED_EDGE('',*,*,#3558,.T.);
#4717=ORIENTED_EDGE('',*,*,#3559,.T.);
#4718=ORIENTED_EDGE('',*,*,#3560,.T.);
#4719=ORIENTED_EDGE('',*,*,#3555,.F.);
#4720=ORIENTED_EDGE('',*,*,#3561,.T.);
#4721=ORIENTED_EDGE('',*,*,#3562,.T.);
#4722=ORIENTED_EDGE('',*,*,#3563,.T.);
#4723=ORIENTED_EDGE('',*,*,#3559,.F.);
#4724=ORIENTED_EDGE('',*,*,#3564,.T.);
#4725=ORIENTED_EDGE('',*,*,#3565,.T.);
#4726=ORIENTED_EDGE('',*,*,#3566,.T.);
#4727=ORIENTED_EDGE('',*,*,#3562,.F.);
#4728=ORIENTED_EDGE('',*,*,#3567,.T.);
#4729=ORIENTED_EDGE('',*,*,#3568,.T.);
#4730=ORIENTED_EDGE('',*,*,#3569,.T.);
#4731=ORIENTED_EDGE('',*,*,#3565,.F.);
#4732=ORIENTED_EDGE('',*,*,#3570,.T.);
#4733=ORIENTED_EDGE('',*,*,#3557,.T.);
#4734=ORIENTED_EDGE('',*,*,#3571,.T.);
#4735=ORIENTED_EDGE('',*,*,#3568,.F.);
#4736=ORIENTED_EDGE('',*,*,#3570,.F.);
#4737=ORIENTED_EDGE('',*,*,#3567,.F.);
#4738=ORIENTED_EDGE('',*,*,#3564,.F.);
#4739=ORIENTED_EDGE('',*,*,#3561,.F.);
#4740=ORIENTED_EDGE('',*,*,#3558,.F.);
#4741=ORIENTED_EDGE('',*,*,#3554,.F.);
#4742=ORIENTED_EDGE('',*,*,#3571,.F.);
#4743=ORIENTED_EDGE('',*,*,#3556,.F.);
#4744=ORIENTED_EDGE('',*,*,#3560,.F.);
#4745=ORIENTED_EDGE('',*,*,#3563,.F.);
#4746=ORIENTED_EDGE('',*,*,#3566,.F.);
#4747=ORIENTED_EDGE('',*,*,#3569,.F.);
#4748=ORIENTED_EDGE('',*,*,#3572,.F.);
#4749=ORIENTED_EDGE('',*,*,#3573,.T.);
#4750=ORIENTED_EDGE('',*,*,#3574,.T.);
#4751=ORIENTED_EDGE('',*,*,#3573,.F.);
#4752=ORIENTED_EDGE('',*,*,#3575,.F.);
#4753=ORIENTED_EDGE('',*,*,#3576,.T.);
#4754=ORIENTED_EDGE('',*,*,#3577,.T.);
#4755=ORIENTED_EDGE('',*,*,#3576,.F.);
#4756=ORIENTED_EDGE('',*,*,#3575,.T.);
#4757=ORIENTED_EDGE('',*,*,#3572,.T.);
#4758=ORIENTED_EDGE('',*,*,#3577,.F.);
#4759=ORIENTED_EDGE('',*,*,#3574,.F.);
#4760=ORIENTED_EDGE('',*,*,#3578,.F.);
#4761=ORIENTED_EDGE('',*,*,#3579,.F.);
#4762=ORIENTED_EDGE('',*,*,#3580,.T.);
#4763=ORIENTED_EDGE('',*,*,#3581,.F.);
#4764=ORIENTED_EDGE('',*,*,#3580,.F.);
#4765=ORIENTED_EDGE('',*,*,#3582,.F.);
#4766=ORIENTED_EDGE('',*,*,#3583,.F.);
#4767=ORIENTED_EDGE('',*,*,#3584,.F.);
#4768=ORIENTED_EDGE('',*,*,#3585,.F.);
#4769=ORIENTED_EDGE('',*,*,#3586,.F.);
#4770=ORIENTED_EDGE('',*,*,#3587,.T.);
#4771=ORIENTED_EDGE('',*,*,#3588,.F.);
#4772=ORIENTED_EDGE('',*,*,#3589,.F.);
#4773=ORIENTED_EDGE('',*,*,#3590,.F.);
#4774=ORIENTED_EDGE('',*,*,#3591,.F.);
#4775=ORIENTED_EDGE('',*,*,#3592,.F.);
#4776=ORIENTED_EDGE('',*,*,#3593,.F.);
#4777=ORIENTED_EDGE('',*,*,#3587,.F.);
#4778=ORIENTED_EDGE('',*,*,#3583,.T.);
#4779=ORIENTED_EDGE('',*,*,#3594,.T.);
#4780=ORIENTED_EDGE('',*,*,#3592,.T.);
#4781=ORIENTED_EDGE('',*,*,#3595,.F.);
#4782=ORIENTED_EDGE('',*,*,#3582,.T.);
#4783=ORIENTED_EDGE('',*,*,#3596,.T.);
#4784=ORIENTED_EDGE('',*,*,#3593,.T.);
#4785=ORIENTED_EDGE('',*,*,#3594,.F.);
#4786=ORIENTED_EDGE('',*,*,#3579,.T.);
#4787=ORIENTED_EDGE('',*,*,#3597,.T.);
#4788=ORIENTED_EDGE('',*,*,#3588,.T.);
#4789=ORIENTED_EDGE('',*,*,#3596,.F.);
#4790=ORIENTED_EDGE('',*,*,#3598,.F.);
#4791=ORIENTED_EDGE('',*,*,#3599,.T.);
#4792=ORIENTED_EDGE('',*,*,#3600,.T.);
#4793=ORIENTED_EDGE('',*,*,#3599,.F.);
#4794=ORIENTED_EDGE('',*,*,#3578,.T.);
#4795=ORIENTED_EDGE('',*,*,#3601,.T.);
#4796=ORIENTED_EDGE('',*,*,#3589,.T.);
#4797=ORIENTED_EDGE('',*,*,#3597,.F.);
#4798=ORIENTED_EDGE('',*,*,#3584,.T.);
#4799=ORIENTED_EDGE('',*,*,#3595,.T.);
#4800=ORIENTED_EDGE('',*,*,#3591,.T.);
#4801=ORIENTED_EDGE('',*,*,#3602,.F.);
#4802=ORIENTED_EDGE('',*,*,#3585,.T.);
#4803=ORIENTED_EDGE('',*,*,#3602,.T.);
#4804=ORIENTED_EDGE('',*,*,#3590,.T.);
#4805=ORIENTED_EDGE('',*,*,#3601,.F.);
#4806=ORIENTED_EDGE('',*,*,#3586,.T.);
#4807=ORIENTED_EDGE('',*,*,#3598,.T.);
#4808=ORIENTED_EDGE('',*,*,#3581,.T.);
#4809=ORIENTED_EDGE('',*,*,#3600,.F.);
#4810=ORIENTED_EDGE('',*,*,#3603,.F.);
#4811=ORIENTED_EDGE('',*,*,#3604,.F.);
#4812=ORIENTED_EDGE('',*,*,#3605,.F.);
#4813=ORIENTED_EDGE('',*,*,#3606,.T.);
#4814=ORIENTED_EDGE('',*,*,#3607,.F.);
#4815=ORIENTED_EDGE('',*,*,#3606,.F.);
#4816=ORIENTED_EDGE('',*,*,#3608,.F.);
#4817=ORIENTED_EDGE('',*,*,#3609,.T.);
#4818=ORIENTED_EDGE('',*,*,#3610,.F.);
#4819=ORIENTED_EDGE('',*,*,#3611,.F.);
#4820=ORIENTED_EDGE('',*,*,#3609,.F.);
#4821=ORIENTED_EDGE('',*,*,#3612,.F.);
#4822=ORIENTED_EDGE('',*,*,#3613,.T.);
#4823=ORIENTED_EDGE('',*,*,#3614,.F.);
#4824=ORIENTED_EDGE('',*,*,#3613,.F.);
#4825=ORIENTED_EDGE('',*,*,#3615,.F.);
#4826=ORIENTED_EDGE('',*,*,#3604,.T.);
#4827=ORIENTED_EDGE('',*,*,#3608,.T.);
#4828=ORIENTED_EDGE('',*,*,#3605,.T.);
#4829=ORIENTED_EDGE('',*,*,#3615,.T.);
#4830=ORIENTED_EDGE('',*,*,#3612,.T.);
#4831=ORIENTED_EDGE('',*,*,#3616,.F.);
#4832=ORIENTED_EDGE('',*,*,#3617,.T.);
#4833=ORIENTED_EDGE('',*,*,#3618,.F.);
#4834=ORIENTED_EDGE('',*,*,#3617,.F.);
#4835=ORIENTED_EDGE('',*,*,#3611,.T.);
#4836=ORIENTED_EDGE('',*,*,#3614,.T.);
#4837=ORIENTED_EDGE('',*,*,#3603,.T.);
#4838=ORIENTED_EDGE('',*,*,#3607,.T.);
#4839=ORIENTED_EDGE('',*,*,#3619,.T.);
#4840=ORIENTED_EDGE('',*,*,#3619,.F.);
#4841=ORIENTED_EDGE('',*,*,#3610,.T.);
#4842=ORIENTED_EDGE('',*,*,#3618,.T.);
#4843=ORIENTED_EDGE('',*,*,#3616,.T.);
#4844=ORIENTED_EDGE('',*,*,#3620,.F.);
#4845=ORIENTED_EDGE('',*,*,#3621,.T.);
#4846=ORIENTED_EDGE('',*,*,#3622,.F.);
#4847=ORIENTED_EDGE('',*,*,#3621,.F.);
#4848=ORIENTED_EDGE('',*,*,#3620,.T.);
#4849=ORIENTED_EDGE('',*,*,#3623,.T.);
#4850=ORIENTED_EDGE('',*,*,#3624,.F.);
#4851=ORIENTED_EDGE('',*,*,#3625,.F.);
#4852=ORIENTED_EDGE('',*,*,#3626,.T.);
#4853=ORIENTED_EDGE('',*,*,#3627,.F.);
#4854=ORIENTED_EDGE('',*,*,#3628,.F.);
#4855=ORIENTED_EDGE('',*,*,#3629,.T.);
#4856=ORIENTED_EDGE('',*,*,#3630,.F.);
#4857=ORIENTED_EDGE('',*,*,#3631,.F.);
#4858=ORIENTED_EDGE('',*,*,#3632,.T.);
#4859=ORIENTED_EDGE('',*,*,#3633,.F.);
#4860=ORIENTED_EDGE('',*,*,#3634,.F.);
#4861=ORIENTED_EDGE('',*,*,#3633,.T.);
#4862=ORIENTED_EDGE('',*,*,#3635,.F.);
#4863=ORIENTED_EDGE('',*,*,#3625,.T.);
#4864=ORIENTED_EDGE('',*,*,#3636,.T.);
#4865=ORIENTED_EDGE('',*,*,#3637,.F.);
#4866=ORIENTED_EDGE('',*,*,#3638,.F.);
#4867=ORIENTED_EDGE('',*,*,#3630,.T.);
#4868=ORIENTED_EDGE('',*,*,#3639,.F.);
#4869=ORIENTED_EDGE('',*,*,#3634,.T.);
#4870=ORIENTED_EDGE('',*,*,#3638,.T.);
#4871=ORIENTED_EDGE('',*,*,#3640,.F.);
#4872=ORIENTED_EDGE('',*,*,#3641,.F.);
#4873=ORIENTED_EDGE('',*,*,#3627,.T.);
#4874=ORIENTED_EDGE('',*,*,#3642,.F.);
#4875=ORIENTED_EDGE('',*,*,#3631,.T.);
#4876=ORIENTED_EDGE('',*,*,#3641,.T.);
#4877=ORIENTED_EDGE('',*,*,#3643,.F.);
#4878=ORIENTED_EDGE('',*,*,#3644,.F.);
#4879=ORIENTED_EDGE('',*,*,#3624,.T.);
#4880=ORIENTED_EDGE('',*,*,#3645,.F.);
#4881=ORIENTED_EDGE('',*,*,#3628,.T.);
#4882=ORIENTED_EDGE('',*,*,#3644,.T.);
#4883=ORIENTED_EDGE('',*,*,#3646,.F.);
#4884=ORIENTED_EDGE('',*,*,#3636,.F.);
#4885=ORIENTED_EDGE('',*,*,#3646,.T.);
#4886=ORIENTED_EDGE('',*,*,#3643,.T.);
#4887=ORIENTED_EDGE('',*,*,#3640,.T.);
#4888=ORIENTED_EDGE('',*,*,#3637,.T.);
#4889=ORIENTED_EDGE('',*,*,#3622,.T.);
#4890=ORIENTED_EDGE('',*,*,#3642,.T.);
#4891=ORIENTED_EDGE('',*,*,#3647,.T.);
#4892=ORIENTED_EDGE('',*,*,#3645,.T.);
#4893=ORIENTED_EDGE('',*,*,#3648,.T.);
#4894=ORIENTED_EDGE('',*,*,#3649,.T.);
#4895=ORIENTED_EDGE('',*,*,#3635,.T.);
#4896=ORIENTED_EDGE('',*,*,#3650,.T.);
#4897=ORIENTED_EDGE('',*,*,#3639,.T.);
#4898=ORIENTED_EDGE('',*,*,#3651,.T.);
#4899=ORIENTED_EDGE('',*,*,#3652,.T.);
#4900=ORIENTED_EDGE('',*,*,#3653,.T.);
#4901=ORIENTED_EDGE('',*,*,#3654,.F.);
#4902=ORIENTED_EDGE('',*,*,#3655,.F.);
#4903=ORIENTED_EDGE('',*,*,#3656,.T.);
#4904=ORIENTED_EDGE('',*,*,#3655,.T.);
#4905=ORIENTED_EDGE('',*,*,#3657,.F.);
#4906=ORIENTED_EDGE('',*,*,#3658,.F.);
#4907=ORIENTED_EDGE('',*,*,#3659,.T.);
#4908=ORIENTED_EDGE('',*,*,#3658,.T.);
#4909=ORIENTED_EDGE('',*,*,#3660,.F.);
#4910=ORIENTED_EDGE('',*,*,#3661,.F.);
#4911=ORIENTED_EDGE('',*,*,#3662,.T.);
#4912=ORIENTED_EDGE('',*,*,#3661,.T.);
#4913=ORIENTED_EDGE('',*,*,#3663,.F.);
#4914=ORIENTED_EDGE('',*,*,#3653,.F.);
#4915=ORIENTED_EDGE('',*,*,#3662,.F.);
#4916=ORIENTED_EDGE('',*,*,#3652,.F.);
#4917=ORIENTED_EDGE('',*,*,#3656,.F.);
#4918=ORIENTED_EDGE('',*,*,#3659,.F.);
#4919=ORIENTED_EDGE('',*,*,#3648,.F.);
#4920=ORIENTED_EDGE('',*,*,#3623,.F.);
#4921=ORIENTED_EDGE('',*,*,#3650,.F.);
#4922=ORIENTED_EDGE('',*,*,#3632,.F.);
#4923=ORIENTED_EDGE('',*,*,#3651,.F.);
#4924=ORIENTED_EDGE('',*,*,#3629,.F.);
#4925=ORIENTED_EDGE('',*,*,#3647,.F.);
#4926=ORIENTED_EDGE('',*,*,#3626,.F.);
#4927=ORIENTED_EDGE('',*,*,#3649,.F.);
#4928=ORIENTED_EDGE('',*,*,#3664,.T.);
#4929=ORIENTED_EDGE('',*,*,#3665,.T.);
#4930=ORIENTED_EDGE('',*,*,#3664,.F.);
#4931=ORIENTED_EDGE('',*,*,#3665,.F.);
#4932=ORIENTED_EDGE('',*,*,#3654,.T.);
#4933=ORIENTED_EDGE('',*,*,#3663,.T.);
#4934=ORIENTED_EDGE('',*,*,#3660,.T.);
#4935=ORIENTED_EDGE('',*,*,#3657,.T.);
#4936=ORIENTED_EDGE('',*,*,#3666,.F.);
#4937=ORIENTED_EDGE('',*,*,#3667,.F.);
#4938=ORIENTED_EDGE('',*,*,#3668,.F.);
#4939=ORIENTED_EDGE('',*,*,#3669,.T.);
#4940=ORIENTED_EDGE('',*,*,#3670,.F.);
#4941=ORIENTED_EDGE('',*,*,#3669,.F.);
#4942=ORIENTED_EDGE('',*,*,#3671,.F.);
#4943=ORIENTED_EDGE('',*,*,#3672,.T.);
#4944=ORIENTED_EDGE('',*,*,#3673,.F.);
#4945=ORIENTED_EDGE('',*,*,#3672,.F.);
#4946=ORIENTED_EDGE('',*,*,#3674,.F.);
#4947=ORIENTED_EDGE('',*,*,#3675,.T.);
#4948=ORIENTED_EDGE('',*,*,#3676,.F.);
#4949=ORIENTED_EDGE('',*,*,#3675,.F.);
#4950=ORIENTED_EDGE('',*,*,#3677,.F.);
#4951=ORIENTED_EDGE('',*,*,#3667,.T.);
#4952=ORIENTED_EDGE('',*,*,#3678,.T.);
#4953=ORIENTED_EDGE('',*,*,#3679,.T.);
#4954=ORIENTED_EDGE('',*,*,#3680,.F.);
#4955=ORIENTED_EDGE('',*,*,#3681,.F.);
#4956=ORIENTED_EDGE('',*,*,#3682,.T.);
#4957=ORIENTED_EDGE('',*,*,#3681,.T.);
#4958=ORIENTED_EDGE('',*,*,#3683,.F.);
#4959=ORIENTED_EDGE('',*,*,#3684,.F.);
#4960=ORIENTED_EDGE('',*,*,#3685,.T.);
#4961=ORIENTED_EDGE('',*,*,#3684,.T.);
#4962=ORIENTED_EDGE('',*,*,#3686,.F.);
#4963=ORIENTED_EDGE('',*,*,#3687,.F.);
#4964=ORIENTED_EDGE('',*,*,#3688,.T.);
#4965=ORIENTED_EDGE('',*,*,#3687,.T.);
#4966=ORIENTED_EDGE('',*,*,#3689,.F.);
#4967=ORIENTED_EDGE('',*,*,#3679,.F.);
#4968=ORIENTED_EDGE('',*,*,#3689,.T.);
#4969=ORIENTED_EDGE('',*,*,#3686,.T.);
#4970=ORIENTED_EDGE('',*,*,#3683,.T.);
#4971=ORIENTED_EDGE('',*,*,#3680,.T.);
#4972=ORIENTED_EDGE('',*,*,#3673,.T.);
#4973=ORIENTED_EDGE('',*,*,#3676,.T.);
#4974=ORIENTED_EDGE('',*,*,#3666,.T.);
#4975=ORIENTED_EDGE('',*,*,#3670,.T.);
#4976=ORIENTED_EDGE('',*,*,#3688,.F.);
#4977=ORIENTED_EDGE('',*,*,#3678,.F.);
#4978=ORIENTED_EDGE('',*,*,#3682,.F.);
#4979=ORIENTED_EDGE('',*,*,#3685,.F.);
#4980=ORIENTED_EDGE('',*,*,#3674,.T.);
#4981=ORIENTED_EDGE('',*,*,#3671,.T.);
#4982=ORIENTED_EDGE('',*,*,#3668,.T.);
#4983=ORIENTED_EDGE('',*,*,#3677,.T.);
#4984=ORIENTED_EDGE('',*,*,#3690,.F.);
#4985=ORIENTED_EDGE('',*,*,#3691,.T.);
#4986=ORIENTED_EDGE('',*,*,#3692,.T.);
#4987=ORIENTED_EDGE('',*,*,#3691,.F.);
#4988=ORIENTED_EDGE('',*,*,#3693,.F.);
#4989=ORIENTED_EDGE('',*,*,#3694,.T.);
#4990=ORIENTED_EDGE('',*,*,#3695,.T.);
#4991=ORIENTED_EDGE('',*,*,#3694,.F.);
#4992=ORIENTED_EDGE('',*,*,#3693,.T.);
#4993=ORIENTED_EDGE('',*,*,#3690,.T.);
#4994=ORIENTED_EDGE('',*,*,#3695,.F.);
#4995=ORIENTED_EDGE('',*,*,#3692,.F.);
#4996=ORIENTED_EDGE('',*,*,#3696,.T.);
#4997=ORIENTED_EDGE('',*,*,#3697,.T.);
#4998=ORIENTED_EDGE('',*,*,#3698,.F.);
#4999=ORIENTED_EDGE('',*,*,#3699,.F.);
#5000=ORIENTED_EDGE('',*,*,#3700,.T.);
#5001=ORIENTED_EDGE('',*,*,#3699,.T.);
#5002=ORIENTED_EDGE('',*,*,#3701,.F.);
#5003=ORIENTED_EDGE('',*,*,#3702,.F.);
#5004=ORIENTED_EDGE('',*,*,#3703,.T.);
#5005=ORIENTED_EDGE('',*,*,#3702,.T.);
#5006=ORIENTED_EDGE('',*,*,#3704,.F.);
#5007=ORIENTED_EDGE('',*,*,#3705,.F.);
#5008=ORIENTED_EDGE('',*,*,#3706,.T.);
#5009=ORIENTED_EDGE('',*,*,#3705,.T.);
#5010=ORIENTED_EDGE('',*,*,#3707,.F.);
#5011=ORIENTED_EDGE('',*,*,#3697,.F.);
#5012=ORIENTED_EDGE('',*,*,#3707,.T.);
#5013=ORIENTED_EDGE('',*,*,#3704,.T.);
#5014=ORIENTED_EDGE('',*,*,#3701,.T.);
#5015=ORIENTED_EDGE('',*,*,#3698,.T.);
#5016=ORIENTED_EDGE('',*,*,#3706,.F.);
#5017=ORIENTED_EDGE('',*,*,#3696,.F.);
#5018=ORIENTED_EDGE('',*,*,#3700,.F.);
#5019=ORIENTED_EDGE('',*,*,#3703,.F.);
#5020=ORIENTED_EDGE('',*,*,#3708,.T.);
#5021=ORIENTED_EDGE('',*,*,#3709,.T.);
#5022=ORIENTED_EDGE('',*,*,#3710,.T.);
#5023=ORIENTED_EDGE('',*,*,#3711,.F.);
#5024=ORIENTED_EDGE('',*,*,#3712,.T.);
#5025=ORIENTED_EDGE('',*,*,#3713,.T.);
#5026=ORIENTED_EDGE('',*,*,#3714,.T.);
#5027=ORIENTED_EDGE('',*,*,#3709,.F.);
#5028=ORIENTED_EDGE('',*,*,#3715,.T.);
#5029=ORIENTED_EDGE('',*,*,#3716,.T.);
#5030=ORIENTED_EDGE('',*,*,#3717,.T.);
#5031=ORIENTED_EDGE('',*,*,#3713,.F.);
#5032=ORIENTED_EDGE('',*,*,#3718,.T.);
#5033=ORIENTED_EDGE('',*,*,#3719,.T.);
#5034=ORIENTED_EDGE('',*,*,#3720,.T.);
#5035=ORIENTED_EDGE('',*,*,#3716,.F.);
#5036=ORIENTED_EDGE('',*,*,#3721,.T.);
#5037=ORIENTED_EDGE('',*,*,#3722,.T.);
#5038=ORIENTED_EDGE('',*,*,#3723,.T.);
#5039=ORIENTED_EDGE('',*,*,#3719,.F.);
#5040=ORIENTED_EDGE('',*,*,#3724,.T.);
#5041=ORIENTED_EDGE('',*,*,#3711,.T.);
#5042=ORIENTED_EDGE('',*,*,#3725,.T.);
#5043=ORIENTED_EDGE('',*,*,#3722,.F.);
#5044=ORIENTED_EDGE('',*,*,#3724,.F.);
#5045=ORIENTED_EDGE('',*,*,#3721,.F.);
#5046=ORIENTED_EDGE('',*,*,#3718,.F.);
#5047=ORIENTED_EDGE('',*,*,#3715,.F.);
#5048=ORIENTED_EDGE('',*,*,#3712,.F.);
#5049=ORIENTED_EDGE('',*,*,#3708,.F.);
#5050=ORIENTED_EDGE('',*,*,#3725,.F.);
#5051=ORIENTED_EDGE('',*,*,#3710,.F.);
#5052=ORIENTED_EDGE('',*,*,#3714,.F.);
#5053=ORIENTED_EDGE('',*,*,#3717,.F.);
#5054=ORIENTED_EDGE('',*,*,#3720,.F.);
#5055=ORIENTED_EDGE('',*,*,#3723,.F.);
#5056=ORIENTED_EDGE('',*,*,#3726,.F.);
#5057=ORIENTED_EDGE('',*,*,#3727,.F.);
#5058=ORIENTED_EDGE('',*,*,#3728,.F.);
#5059=ORIENTED_EDGE('',*,*,#3729,.T.);
#5060=ORIENTED_EDGE('',*,*,#3727,.T.);
#5061=ORIENTED_EDGE('',*,*,#3729,.F.);
#5062=ORIENTED_EDGE('',*,*,#3730,.F.);
#5063=ORIENTED_EDGE('',*,*,#3731,.T.);
#5064=ORIENTED_EDGE('',*,*,#3728,.T.);
#5065=ORIENTED_EDGE('',*,*,#3731,.F.);
#5066=ORIENTED_EDGE('',*,*,#3732,.F.);
#5067=ORIENTED_EDGE('',*,*,#3733,.T.);
#5068=ORIENTED_EDGE('',*,*,#3730,.T.);
#5069=ORIENTED_EDGE('',*,*,#3733,.F.);
#5070=ORIENTED_EDGE('',*,*,#3732,.T.);
#5071=ORIENTED_EDGE('',*,*,#3734,.F.);
#5072=ORIENTED_EDGE('',*,*,#3735,.F.);
#5073=ORIENTED_EDGE('',*,*,#3736,.T.);
#5074=ORIENTED_EDGE('',*,*,#3734,.T.);
#5075=ORIENTED_EDGE('',*,*,#3736,.F.);
#5076=ORIENTED_EDGE('',*,*,#3726,.T.);
#5077=ORIENTED_EDGE('',*,*,#3737,.T.);
#5078=ORIENTED_EDGE('',*,*,#3735,.T.);
#5079=ORIENTED_EDGE('',*,*,#3737,.F.);
#5080=CYLINDRICAL_SURFACE('',#5909,0.165);
#5081=CYLINDRICAL_SURFACE('',#5913,0.165);
#5082=CYLINDRICAL_SURFACE('',#5917,0.275);
#5083=CYLINDRICAL_SURFACE('',#5920,0.275);
#5084=CYLINDRICAL_SURFACE('',#5923,0.275);
#5085=CYLINDRICAL_SURFACE('',#5926,0.275);
#5086=CYLINDRICAL_SURFACE('',#5929,0.7);
#5087=CYLINDRICAL_SURFACE('',#5935,0.93);
#5088=CYLINDRICAL_SURFACE('',#5938,1.3);
#5089=CYLINDRICAL_SURFACE('',#5952,0.165);
#5090=CYLINDRICAL_SURFACE('',#5956,0.165);
#5091=CYLINDRICAL_SURFACE('',#5960,0.275);
#5092=CYLINDRICAL_SURFACE('',#5963,0.275);
#5093=CYLINDRICAL_SURFACE('',#5966,0.275);
#5094=CYLINDRICAL_SURFACE('',#5969,0.275);
#5095=CYLINDRICAL_SURFACE('',#5972,0.7);
#5096=CYLINDRICAL_SURFACE('',#5978,0.93);
#5097=CYLINDRICAL_SURFACE('',#5981,1.3);
#5098=CYLINDRICAL_SURFACE('',#5995,0.275);
#5099=CYLINDRICAL_SURFACE('',#5998,0.275);
#5100=CYLINDRICAL_SURFACE('',#6001,0.275);
#5101=CYLINDRICAL_SURFACE('',#6004,0.275);
#5102=CYLINDRICAL_SURFACE('',#6015,1.6);
#5103=CYLINDRICAL_SURFACE('',#6025,1.2);
#5104=CYLINDRICAL_SURFACE('',#6029,0.405);
#5105=CYLINDRICAL_SURFACE('',#6031,0.7);
#5106=CYLINDRICAL_SURFACE('',#6039,0.61);
#5107=CYLINDRICAL_SURFACE('',#6044,0.405);
#5108=CYLINDRICAL_SURFACE('',#6046,1.);
#5109=CYLINDRICAL_SURFACE('',#6052,0.3);
#5110=CYLINDRICAL_SURFACE('',#6056,0.3);
#5111=CYLINDRICAL_SURFACE('',#6060,0.225);
#5112=CYLINDRICAL_SURFACE('',#6063,0.225);
#5113=CYLINDRICAL_SURFACE('',#6066,0.225);
#5114=CYLINDRICAL_SURFACE('',#6069,0.225);
#5115=CYLINDRICAL_SURFACE('',#6072,1.01);
#5116=CYLINDRICAL_SURFACE('',#6085,0.75);
#5117=CYLINDRICAL_SURFACE('',#6087,1.3);
#5118=CYLINDRICAL_SURFACE('',#6104,0.25);
#5119=CYLINDRICAL_SURFACE('',#6111,0.425);
#5120=CYLINDRICAL_SURFACE('',#6119,0.24505);
#5121=CYLINDRICAL_SURFACE('',#6124,0.265);
#5122=CYLINDRICAL_SURFACE('',#6128,0.5);
#5123=CYLINDRICAL_SURFACE('',#6139,0.2117);
#5124=CYLINDRICAL_SURFACE('',#6148,0.225);
#5125=CYLINDRICAL_SURFACE('',#6151,0.4);
#5126=CYLINDRICAL_SURFACE('',#6161,0.35);
#5127=CYLINDRICAL_SURFACE('',#6169,0.1954);
#5128=CYLINDRICAL_SURFACE('',#6183,0.3);
#5129=CYLINDRICAL_SURFACE('',#6224,0.79);
#5130=CYLINDRICAL_SURFACE('',#6227,2.2);
#5131=CYLINDRICAL_SURFACE('',#6236,0.93);
#5132=CYLINDRICAL_SURFACE('',#6244,0.93);
#5133=CYLINDRICAL_SURFACE('',#6248,0.789999999999999);
#5134=CYLINDRICAL_SURFACE('',#6253,0.789999999999999);
#5135=CYLINDRICAL_SURFACE('',#6260,0.93);
#5136=CYLINDRICAL_SURFACE('',#6262,0.79);
#5137=CYLINDRICAL_SURFACE('',#6269,0.789999999999999);
#5138=CYLINDRICAL_SURFACE('',#6271,0.789999999999999);
#5139=CYLINDRICAL_SURFACE('',#6273,1.6);
#5140=CYLINDRICAL_SURFACE('',#6279,1.6);
#5141=CYLINDRICAL_SURFACE('',#6285,0.79);
#5142=CYLINDRICAL_SURFACE('',#6288,1.065);
#5143=CYLINDRICAL_SURFACE('',#6294,0.789999999999999);
#5144=CYLINDRICAL_SURFACE('',#6297,1.065);
#5145=CYLINDRICAL_SURFACE('',#6303,0.79);
#5146=CYLINDRICAL_SURFACE('',#6306,1.065);
#5147=CYLINDRICAL_SURFACE('',#6312,0.79);
#5148=CYLINDRICAL_SURFACE('',#6321,0.79);
#5149=CYLINDRICAL_SURFACE('',#6325,0.93);
#5150=CYLINDRICAL_SURFACE('',#6327,0.93);
#5151=CYLINDRICAL_SURFACE('',#6336,1.2);
#5152=CYLINDRICAL_SURFACE('',#6341,1.45);
#5153=CYLINDRICAL_SURFACE('',#6347,1.45);
#5154=CYLINDRICAL_SURFACE('',#6350,1.2);
#5155=CYLINDRICAL_SURFACE('',#6362,1.065);
#5156=CYLINDRICAL_SURFACE('',#6368,1.065);
#5157=CYLINDRICAL_SURFACE('',#6374,0.79);
#5158=CYLINDRICAL_SURFACE('',#6376,0.44);
#5159=CYLINDRICAL_SURFACE('',#6379,0.44);
#5160=CYLINDRICAL_SURFACE('',#6382,0.44);
#5161=CYLINDRICAL_SURFACE('',#6385,0.44);
#5162=CYLINDRICAL_SURFACE('',#6391,3.5);
#5163=CYLINDRICAL_SURFACE('',#6393,0.79);
#5164=CYLINDRICAL_SURFACE('',#6396,1.5);
#5165=CYLINDRICAL_SURFACE('',#6401,0.44);
#5166=CYLINDRICAL_SURFACE('',#6404,0.44);
#5167=CYLINDRICAL_SURFACE('',#6407,0.44);
#5168=CYLINDRICAL_SURFACE('',#6410,0.44);
#5169=CYLINDRICAL_SURFACE('',#6416,3.5);
#5170=CYLINDRICAL_SURFACE('',#6418,0.79);
#5171=CYLINDRICAL_SURFACE('',#6421,1.5);
#5172=CYLINDRICAL_SURFACE('',#6430,0.65);
#5173=CYLINDRICAL_SURFACE('',#6438,0.3933);
#5174=CYLINDRICAL_SURFACE('',#6452,0.42);
#5175=CYLINDRICAL_SURFACE('',#6455,0.8);
#5176=CYLINDRICAL_SURFACE('',#6468,0.338975);
#5177=CYLINDRICAL_SURFACE('',#6520,0.75);
#5178=CYLINDRICAL_SURFACE('',#6526,0.165);
#5179=CYLINDRICAL_SURFACE('',#6557,0.4);
#5180=CYLINDRICAL_SURFACE('',#6572,0.225);
#5181=CYLINDRICAL_SURFACE('',#6575,0.6);
#5182=CYLINDRICAL_SURFACE('',#6602,0.35);
#5183=CYLINDRICAL_SURFACE('',#6610,0.1954);
#5184=ADVANCED_FACE('',(#835),#5080,.F.);
#5185=ADVANCED_FACE('',(#836),#635,.T.);
#5186=ADVANCED_FACE('',(#837),#5081,.F.);
#5187=ADVANCED_FACE('',(#838),#636,.T.);
#5188=ADVANCED_FACE('',(#839),#5082,.F.);
#5189=ADVANCED_FACE('',(#840),#5083,.F.);
#5190=ADVANCED_FACE('',(#841),#5084,.F.);
#5191=ADVANCED_FACE('',(#842),#5085,.F.);
#5192=ADVANCED_FACE('',(#843),#5086,.F.);
#5193=ADVANCED_FACE('',(#844),#637,.T.);
#5194=ADVANCED_FACE('',(#845,#511,#512),#638,.T.);
#5195=ADVANCED_FACE('',(#846),#5087,.F.);
#5196=ADVANCED_FACE('',(#847),#5088,.F.);
#5197=ADVANCED_FACE('',(#848,#513),#639,.F.);
#5198=ADVANCED_FACE('',(#849,#514),#640,.T.);
#5199=ADVANCED_FACE('',(#850,#515),#505,.F.);
#5200=ADVANCED_FACE('',(#851,#516,#517,#518,#519),#641,.T.);
#5201=ADVANCED_FACE('',(#852),#642,.T.);
#5202=ADVANCED_FACE('',(#853,#520,#521,#522,#523,#524),#643,.T.);
#5203=ADVANCED_FACE('',(#854),#644,.T.);
#5204=ADVANCED_FACE('',(#855),#645,.F.);
#5205=ADVANCED_FACE('',(#856),#5089,.F.);
#5206=ADVANCED_FACE('',(#857),#646,.T.);
#5207=ADVANCED_FACE('',(#858),#5090,.F.);
#5208=ADVANCED_FACE('',(#859),#647,.T.);
#5209=ADVANCED_FACE('',(#860),#5091,.F.);
#5210=ADVANCED_FACE('',(#861),#5092,.F.);
#5211=ADVANCED_FACE('',(#862),#5093,.F.);
#5212=ADVANCED_FACE('',(#863),#5094,.F.);
#5213=ADVANCED_FACE('',(#864),#5095,.F.);
#5214=ADVANCED_FACE('',(#865),#648,.T.);
#5215=ADVANCED_FACE('',(#866,#525,#526),#649,.T.);
#5216=ADVANCED_FACE('',(#867),#5096,.F.);
#5217=ADVANCED_FACE('',(#868),#5097,.F.);
#5218=ADVANCED_FACE('',(#869,#527),#650,.F.);
#5219=ADVANCED_FACE('',(#870,#528),#651,.T.);
#5220=ADVANCED_FACE('',(#871,#529),#506,.F.);
#5221=ADVANCED_FACE('',(#872,#530,#531,#532,#533,#534),#652,.T.);
#5222=ADVANCED_FACE('',(#873),#653,.T.);
#5223=ADVANCED_FACE('',(#874,#535,#536,#537,#538),#654,.T.);
#5224=ADVANCED_FACE('',(#875),#655,.T.);
#5225=ADVANCED_FACE('',(#876),#656,.F.);
#5226=ADVANCED_FACE('',(#877),#5098,.F.);
#5227=ADVANCED_FACE('',(#878),#5099,.F.);
#5228=ADVANCED_FACE('',(#879),#5100,.F.);
#5229=ADVANCED_FACE('',(#880),#5101,.F.);
#5230=ADVANCED_FACE('',(#881),#657,.F.);
#5231=ADVANCED_FACE('',(#882),#658,.F.);
#5232=ADVANCED_FACE('',(#883),#659,.F.);
#5233=ADVANCED_FACE('',(#884),#660,.F.);
#5234=ADVANCED_FACE('',(#885,#539,#540,#541,#542),#661,.T.);
#5235=ADVANCED_FACE('',(#886),#662,.T.);
#5236=ADVANCED_FACE('',(#887),#663,.T.);
#5237=ADVANCED_FACE('',(#888),#5102,.F.);
#5238=ADVANCED_FACE('',(#889),#664,.T.);
#5239=ADVANCED_FACE('',(#890),#665,.T.);
#5240=ADVANCED_FACE('',(#891),#666,.T.);
#5241=ADVANCED_FACE('',(#892,#543,#544,#545,#546),#667,.F.);
#5242=ADVANCED_FACE('',(#893,#547),#668,.F.);
#5243=ADVANCED_FACE('',(#894),#5103,.T.);
#5244=ADVANCED_FACE('',(#895,#548),#669,.T.);
#5245=ADVANCED_FACE('',(#896),#5104,.F.);
#5246=ADVANCED_FACE('',(#897),#5105,.T.);
#5247=ADVANCED_FACE('',(#898,#549),#670,.F.);
#5248=ADVANCED_FACE('',(#899),#380,.T.);
#5249=ADVANCED_FACE('',(#900),#5106,.F.);
#5250=ADVANCED_FACE('',(#901,#550),#671,.F.);
#5251=ADVANCED_FACE('',(#902),#5107,.F.);
#5252=ADVANCED_FACE('',(#903),#5108,.T.);
#5253=ADVANCED_FACE('',(#904,#551),#672,.T.);
#5254=ADVANCED_FACE('',(#905,#552),#673,.F.);
#5255=ADVANCED_FACE('',(#906),#5109,.F.);
#5256=ADVANCED_FACE('',(#907),#674,.T.);
#5257=ADVANCED_FACE('',(#908),#5110,.F.);
#5258=ADVANCED_FACE('',(#909),#675,.T.);
#5259=ADVANCED_FACE('',(#910),#5111,.F.);
#5260=ADVANCED_FACE('',(#911),#5112,.F.);
#5261=ADVANCED_FACE('',(#912),#5113,.F.);
#5262=ADVANCED_FACE('',(#913),#5114,.F.);
#5263=ADVANCED_FACE('',(#914),#5115,.F.);
#5264=ADVANCED_FACE('',(#915),#676,.T.);
#5265=ADVANCED_FACE('',(#916),#677,.T.);
#5266=ADVANCED_FACE('',(#917),#678,.T.);
#5267=ADVANCED_FACE('',(#918),#679,.T.);
#5268=ADVANCED_FACE('',(#919,#553,#554,#555,#556,#557,#558,#559),#680,.T.);
#5269=ADVANCED_FACE('',(#920,#560,#561,#562,#563,#564),#681,.F.);
#5270=ADVANCED_FACE('',(#921,#565),#507,.F.);
#5271=ADVANCED_FACE('',(#922),#5116,.F.);
#5272=ADVANCED_FACE('',(#923),#5117,.T.);
#5273=ADVANCED_FACE('',(#924,#566),#682,.T.);
#5274=ADVANCED_FACE('',(#925,#567),#683,.F.);
#5275=ADVANCED_FACE('',(#926),#684,.F.);
#5276=ADVANCED_FACE('',(#927),#685,.F.);
#5277=ADVANCED_FACE('',(#928),#686,.F.);
#5278=ADVANCED_FACE('',(#929),#687,.F.);
#5279=ADVANCED_FACE('',(#930),#688,.F.);
#5280=ADVANCED_FACE('',(#931),#689,.F.);
#5281=ADVANCED_FACE('',(#932),#690,.F.);
#5282=ADVANCED_FACE('',(#933),#691,.F.);
#5283=ADVANCED_FACE('',(#934,#568),#692,.T.);
#5284=ADVANCED_FACE('',(#935),#5118,.T.);
#5285=ADVANCED_FACE('',(#936),#693,.F.);
#5286=ADVANCED_FACE('',(#937),#694,.T.);
#5287=ADVANCED_FACE('',(#938),#351,.T.);
#5288=ADVANCED_FACE('',(#939),#5119,.T.);
#5289=ADVANCED_FACE('',(#940),#352,.T.);
#5290=ADVANCED_FACE('',(#941,#569),#695,.T.);
#5291=ADVANCED_FACE('',(#942),#353,.T.);
#5292=ADVANCED_FACE('',(#943),#5120,.T.);
#5293=ADVANCED_FACE('',(#944),#354,.F.);
#5294=ADVANCED_FACE('',(#945),#5121,.F.);
#5295=ADVANCED_FACE('',(#946,#570),#696,.T.);
#5296=ADVANCED_FACE('',(#947),#5122,.T.);
#5297=ADVANCED_FACE('',(#948,#571),#697,.F.);
#5298=ADVANCED_FACE('',(#949),#355,.T.);
#5299=ADVANCED_FACE('',(#950),#356,.T.);
#5300=ADVANCED_FACE('',(#951),#698,.T.);
#5301=ADVANCED_FACE('',(#952),#699,.T.);
#5302=ADVANCED_FACE('',(#953),#700,.T.);
#5303=ADVANCED_FACE('',(#954),#5123,.F.);
#5304=ADVANCED_FACE('',(#955),#701,.T.);
#5305=ADVANCED_FACE('',(#956),#702,.T.);
#5306=ADVANCED_FACE('',(#957),#703,.T.);
#5307=ADVANCED_FACE('',(#958,#572),#704,.T.);
#5308=ADVANCED_FACE('',(#959,#573),#705,.F.);
#5309=ADVANCED_FACE('',(#960),#5124,.F.);
#5310=ADVANCED_FACE('',(#961),#5125,.T.);
#5311=ADVANCED_FACE('',(#962,#574),#706,.T.);
#5312=ADVANCED_FACE('',(#963,#575),#707,.F.);
#5313=ADVANCED_FACE('',(#964),#708,.T.);
#5314=ADVANCED_FACE('',(#965),#357,.T.);
#5315=ADVANCED_FACE('',(#966),#5126,.T.);
#5316=ADVANCED_FACE('',(#967),#358,.T.);
#5317=ADVANCED_FACE('',(#968,#576),#709,.T.);
#5318=ADVANCED_FACE('',(#969),#359,.T.);
#5319=ADVANCED_FACE('',(#970),#5127,.T.);
#5320=ADVANCED_FACE('',(#971),#360,.T.);
#5321=ADVANCED_FACE('',(#972),#710,.T.);
#5322=ADVANCED_FACE('',(#973),#711,.F.);
#5323=ADVANCED_FACE('',(#974),#712,.F.);
#5324=ADVANCED_FACE('',(#975),#713,.F.);
#5325=ADVANCED_FACE('',(#976),#714,.F.);
#5326=ADVANCED_FACE('',(#977),#715,.F.);
#5327=ADVANCED_FACE('',(#978),#716,.F.);
#5328=ADVANCED_FACE('',(#979),#717,.F.);
#5329=ADVANCED_FACE('',(#980),#718,.F.);
#5330=ADVANCED_FACE('',(#981),#5128,.T.);
#5331=ADVANCED_FACE('',(#982),#719,.T.);
#5332=ADVANCED_FACE('',(#983),#720,.F.);
#5333=ADVANCED_FACE('',(#984),#5129,.F.);
#5334=ADVANCED_FACE('',(#985),#5130,.T.);
#5335=ADVANCED_FACE('',(#986,#577),#721,.T.);
#5336=ADVANCED_FACE('',(#987,#578),#722,.F.);
#5337=ADVANCED_FACE('',(#988),#723,.F.);
#5338=ADVANCED_FACE('',(#989),#5131,.F.);
#5339=ADVANCED_FACE('',(#990),#724,.F.);
#5340=ADVANCED_FACE('',(#991),#5132,.F.);
#5341=ADVANCED_FACE('',(#992),#5133,.F.);
#5342=ADVANCED_FACE('',(#993),#725,.T.);
#5343=ADVANCED_FACE('',(#994),#5134,.F.);
#5344=ADVANCED_FACE('',(#995),#726,.F.);
#5345=ADVANCED_FACE('',(#996),#5135,.F.);
#5346=ADVANCED_FACE('',(#997),#5136,.F.);
#5347=ADVANCED_FACE('',(#998),#727,.F.);
#5348=ADVANCED_FACE('',(#999),#5137,.F.);
#5349=ADVANCED_FACE('',(#1000),#5138,.F.);
#5350=ADVANCED_FACE('',(#1001),#728,.F.);
#5351=ADVANCED_FACE('',(#1002),#5139,.T.);
#5352=ADVANCED_FACE('',(#1003,#579),#729,.F.);
#5353=ADVANCED_FACE('',(#1004),#5140,.T.);
#5354=ADVANCED_FACE('',(#1005,#580),#730,.T.);
#5355=ADVANCED_FACE('',(#1006,#581),#731,.F.);
#5356=ADVANCED_FACE('',(#1007),#5141,.F.);
#5357=ADVANCED_FACE('',(#1008),#5142,.T.);
#5358=ADVANCED_FACE('',(#1009,#582),#732,.T.);
#5359=ADVANCED_FACE('',(#1010,#583),#733,.F.);
#5360=ADVANCED_FACE('',(#1011),#5143,.F.);
#5361=ADVANCED_FACE('',(#1012),#5144,.T.);
#5362=ADVANCED_FACE('',(#1013,#584),#734,.T.);
#5363=ADVANCED_FACE('',(#1014,#585),#735,.F.);
#5364=ADVANCED_FACE('',(#1015),#5145,.F.);
#5365=ADVANCED_FACE('',(#1016),#5146,.T.);
#5366=ADVANCED_FACE('',(#1017,#586),#736,.T.);
#5367=ADVANCED_FACE('',(#1018,#587),#737,.F.);
#5368=ADVANCED_FACE('',(#1019),#5147,.F.);
#5369=ADVANCED_FACE('',(#1020,#588),#508,.F.);
#5370=ADVANCED_FACE('',(#1021),#5148,.F.);
#5371=ADVANCED_FACE('',(#1022,#589),#738,.F.);
#5372=ADVANCED_FACE('',(#1023),#5149,.F.);
#5373=ADVANCED_FACE('',(#1024),#5150,.F.);
#5374=ADVANCED_FACE('',(#1025,#590),#739,.F.);
#5375=ADVANCED_FACE('',(#1026),#509,.T.);
#5376=ADVANCED_FACE('',(#1027),#5151,.T.);
#5377=ADVANCED_FACE('',(#1028,#591),#740,.T.);
#5378=ADVANCED_FACE('',(#1029),#5152,.T.);
#5379=ADVANCED_FACE('',(#1030,#592),#741,.T.);
#5380=ADVANCED_FACE('',(#1031,#593),#742,.T.);
#5381=ADVANCED_FACE('',(#1032),#5153,.T.);
#5382=ADVANCED_FACE('',(#1033,#594),#743,.T.);
#5383=ADVANCED_FACE('',(#1034),#5154,.T.);
#5384=ADVANCED_FACE('',(#1035,#595),#744,.F.);
#5385=ADVANCED_FACE('',(#1036,#596),#745,.T.);
#5386=ADVANCED_FACE('',(#1037),#746,.T.);
#5387=ADVANCED_FACE('',(#1038),#747,.T.);
#5388=ADVANCED_FACE('',(#1039),#748,.T.);
#5389=ADVANCED_FACE('',(#1040),#749,.T.);
#5390=ADVANCED_FACE('',(#1041),#750,.T.);
#5391=ADVANCED_FACE('',(#1042),#751,.T.);
#5392=ADVANCED_FACE('',(#1043),#5155,.T.);
#5393=ADVANCED_FACE('',(#1044,#597),#752,.T.);
#5394=ADVANCED_FACE('',(#1045),#361,.T.);
#5395=ADVANCED_FACE('',(#1046),#5156,.T.);
#5396=ADVANCED_FACE('',(#1047),#362,.T.);
#5397=ADVANCED_FACE('',(#1048,#598),#753,.T.);
#5398=ADVANCED_FACE('',(#1049),#5157,.F.);
#5399=ADVANCED_FACE('',(#1050),#5158,.F.);
#5400=ADVANCED_FACE('',(#1051),#5159,.F.);
#5401=ADVANCED_FACE('',(#1052),#5160,.F.);
#5402=ADVANCED_FACE('',(#1053),#5161,.F.);
#5403=ADVANCED_FACE('',(#1054,#599,#600,#601,#602,#603),#754,.F.);
#5404=ADVANCED_FACE('',(#1055),#5162,.T.);
#5405=ADVANCED_FACE('',(#1056),#5163,.F.);
#5406=ADVANCED_FACE('',(#1057),#5164,.T.);
#5407=ADVANCED_FACE('',(#1058,#604,#605,#606,#607,#608),#755,.T.);
#5408=ADVANCED_FACE('',(#1059,#609),#756,.F.);
#5409=ADVANCED_FACE('',(#1060),#5165,.F.);
#5410=ADVANCED_FACE('',(#1061),#5166,.F.);
#5411=ADVANCED_FACE('',(#1062),#5167,.F.);
#5412=ADVANCED_FACE('',(#1063),#5168,.F.);
#5413=ADVANCED_FACE('',(#1064,#610,#611,#612,#613,#614),#757,.T.);
#5414=ADVANCED_FACE('',(#1065),#5169,.T.);
#5415=ADVANCED_FACE('',(#1066),#5170,.F.);
#5416=ADVANCED_FACE('',(#1067),#5171,.T.);
#5417=ADVANCED_FACE('',(#1068,#615),#758,.T.);
#5418=ADVANCED_FACE('',(#1069,#616,#617,#618,#619,#620),#759,.F.);
#5419=ADVANCED_FACE('',(#1070),#760,.T.);
#5420=ADVANCED_FACE('',(#1071),#363,.T.);
#5421=ADVANCED_FACE('',(#1072),#5172,.T.);
#5422=ADVANCED_FACE('',(#1073),#364,.T.);
#5423=ADVANCED_FACE('',(#1074,#621),#761,.T.);
#5424=ADVANCED_FACE('',(#1075),#365,.T.);
#5425=ADVANCED_FACE('',(#1076),#5173,.T.);
#5426=ADVANCED_FACE('',(#1077),#366,.T.);
#5427=ADVANCED_FACE('',(#1078),#762,.T.);
#5428=ADVANCED_FACE('',(#1079),#763,.F.);
#5429=ADVANCED_FACE('',(#1080),#764,.F.);
#5430=ADVANCED_FACE('',(#1081),#765,.F.);
#5431=ADVANCED_FACE('',(#1082),#766,.F.);
#5432=ADVANCED_FACE('',(#1083),#767,.F.);
#5433=ADVANCED_FACE('',(#1084),#768,.F.);
#5434=ADVANCED_FACE('',(#1085),#769,.F.);
#5435=ADVANCED_FACE('',(#1086),#770,.F.);
#5436=ADVANCED_FACE('',(#1087),#5174,.F.);
#5437=ADVANCED_FACE('',(#1088),#5175,.T.);
#5438=ADVANCED_FACE('',(#1089,#622),#771,.T.);
#5439=ADVANCED_FACE('',(#1090,#623),#772,.F.);
#5440=ADVANCED_FACE('',(#1091),#367,.T.);
#5441=ADVANCED_FACE('',(#1092),#368,.T.);
#5442=ADVANCED_FACE('',(#1093),#773,.T.);
#5443=ADVANCED_FACE('',(#1094),#774,.T.);
#5444=ADVANCED_FACE('',(#1095),#775,.T.);
#5445=ADVANCED_FACE('',(#1096),#5176,.F.);
#5446=ADVANCED_FACE('',(#1097),#776,.T.);
#5447=ADVANCED_FACE('',(#1098),#777,.T.);
#5448=ADVANCED_FACE('',(#1099),#778,.T.);
#5449=ADVANCED_FACE('',(#1100,#624),#779,.T.);
#5450=ADVANCED_FACE('',(#1101,#625),#780,.F.);
#5451=ADVANCED_FACE('',(#1102),#781,.F.);
#5452=ADVANCED_FACE('',(#1103),#782,.F.);
#5453=ADVANCED_FACE('',(#1104),#783,.F.);
#5454=ADVANCED_FACE('',(#1105),#784,.F.);
#5455=ADVANCED_FACE('',(#1106),#785,.T.);
#5456=ADVANCED_FACE('',(#1107),#5177,.F.);
#5457=ADVANCED_FACE('',(#1108,#626,#627),#510,.T.);
#5458=ADVANCED_FACE('',(#1109),#5178,.F.);
#5459=ADVANCED_FACE('',(#1110),#786,.T.);
#5460=ADVANCED_FACE('',(#1111),#787,.F.);
#5461=ADVANCED_FACE('',(#1112),#788,.F.);
#5462=ADVANCED_FACE('',(#1113),#789,.F.);
#5463=ADVANCED_FACE('',(#1114),#790,.F.);
#5464=ADVANCED_FACE('',(#1115),#791,.T.);
#5465=ADVANCED_FACE('',(#1116),#792,.T.);
#5466=ADVANCED_FACE('',(#1117),#793,.T.);
#5467=ADVANCED_FACE('',(#1118),#794,.T.);
#5468=ADVANCED_FACE('',(#1119,#628),#795,.T.);
#5469=ADVANCED_FACE('',(#1120),#796,.T.);
#5470=ADVANCED_FACE('',(#1121),#797,.T.);
#5471=ADVANCED_FACE('',(#1122),#798,.T.);
#5472=ADVANCED_FACE('',(#1123),#799,.T.);
#5473=ADVANCED_FACE('',(#1124),#800,.T.);
#5474=ADVANCED_FACE('',(#1125),#801,.T.);
#5475=ADVANCED_FACE('',(#1126),#802,.T.);
#5476=ADVANCED_FACE('',(#1127),#803,.T.);
#5477=ADVANCED_FACE('',(#1128),#804,.F.);
#5478=ADVANCED_FACE('',(#1129),#5179,.T.);
#5479=ADVANCED_FACE('',(#1130,#629),#805,.F.);
#5480=ADVANCED_FACE('',(#1131),#806,.F.);
#5481=ADVANCED_FACE('',(#1132),#807,.F.);
#5482=ADVANCED_FACE('',(#1133),#808,.F.);
#5483=ADVANCED_FACE('',(#1134),#809,.F.);
#5484=ADVANCED_FACE('',(#1135),#810,.T.);
#5485=ADVANCED_FACE('',(#1136),#811,.T.);
#5486=ADVANCED_FACE('',(#1137),#812,.T.);
#5487=ADVANCED_FACE('',(#1138),#813,.T.);
#5488=ADVANCED_FACE('',(#1139,#630),#814,.T.);
#5489=ADVANCED_FACE('',(#1140,#631),#815,.F.);
#5490=ADVANCED_FACE('',(#1141),#5180,.F.);
#5491=ADVANCED_FACE('',(#1142),#5181,.T.);
#5492=ADVANCED_FACE('',(#1143,#632),#816,.T.);
#5493=ADVANCED_FACE('',(#1144,#633),#817,.F.);
#5494=ADVANCED_FACE('',(#1145),#818,.T.);
#5495=ADVANCED_FACE('',(#1146),#819,.T.);
#5496=ADVANCED_FACE('',(#1147),#820,.T.);
#5497=ADVANCED_FACE('',(#1148),#821,.T.);
#5498=ADVANCED_FACE('',(#1149),#822,.T.);
#5499=ADVANCED_FACE('',(#1150),#823,.F.);
#5500=ADVANCED_FACE('',(#1151),#824,.F.);
#5501=ADVANCED_FACE('',(#1152),#825,.F.);
#5502=ADVANCED_FACE('',(#1153),#826,.F.);
#5503=ADVANCED_FACE('',(#1154),#827,.F.);
#5504=ADVANCED_FACE('',(#1155),#828,.F.);
#5505=ADVANCED_FACE('',(#1156),#829,.F.);
#5506=ADVANCED_FACE('',(#1157),#830,.F.);
#5507=ADVANCED_FACE('',(#1158),#831,.F.);
#5508=ADVANCED_FACE('',(#1159),#832,.F.);
#5509=ADVANCED_FACE('',(#1160),#833,.T.);
#5510=ADVANCED_FACE('',(#1161),#369,.T.);
#5511=ADVANCED_FACE('',(#1162),#5182,.T.);
#5512=ADVANCED_FACE('',(#1163),#370,.T.);
#5513=ADVANCED_FACE('',(#1164,#634),#834,.T.);
#5514=ADVANCED_FACE('',(#1165),#371,.T.);
#5515=ADVANCED_FACE('',(#1166),#5183,.T.);
#5516=CLOSED_SHELL('',(#5184,#5185,#5186,#5187,#5188,#5189,#5190,#5191,
#5192,#5193,#5194,#5195,#5196,#5197,#5198,#5199,#5200,#5201,#5202,#5203,
#5204));
#5517=CLOSED_SHELL('',(#5205,#5206,#5207,#5208,#5209,#5210,#5211,#5212,
#5213,#5214,#5215,#5216,#5217,#5218,#5219,#5220,#5221,#5222,#5223,#5224,
#5225));
#5518=CLOSED_SHELL('',(#5226,#5227,#5228,#5229,#5230,#5231,#5232,#5233,
#5234,#5235,#5236,#5237,#5238,#5239,#5240,#5241));
#5519=CLOSED_SHELL('',(#5242,#5243,#5244,#5245,#5246,#5247));
#5520=CLOSED_SHELL('',(#5248));
#5521=CLOSED_SHELL('',(#5249,#5250,#5251,#5252,#5253,#5254));
#5522=CLOSED_SHELL('',(#5255,#5256,#5257,#5258,#5259,#5260,#5261,#5262,
#5263,#5264,#5265,#5266,#5267,#5268,#5269));
#5523=CLOSED_SHELL('',(#5270,#5271,#5272,#5273,#5274));
#5524=CLOSED_SHELL('',(#5275,#5276,#5277,#5278,#5279,#5280,#5281,#5282));
#5525=CLOSED_SHELL('',(#5283,#5284,#5285,#5286,#5287,#5288,#5289,#5290,
#5291,#5292));
#5526=CLOSED_SHELL('',(#5293,#5294,#5295,#5296,#5297));
#5527=CLOSED_SHELL('',(#5298,#5299,#5300,#5301,#5302,#5303,#5304,#5305,
#5306,#5307,#5308));
#5528=CLOSED_SHELL('',(#5309,#5310,#5311,#5312));
#5529=CLOSED_SHELL('',(#5313,#5314,#5315,#5316,#5317,#5318,#5319,#5320,
#5321));
#5530=CLOSED_SHELL('',(#5322,#5323,#5324,#5325,#5326,#5327,#5328,#5329));
#5531=CLOSED_SHELL('',(#5330,#5331,#5332));
#5532=CLOSED_SHELL('',(#5333,#5334,#5335,#5336));
#5533=CLOSED_SHELL('',(#5337,#5338,#5339,#5340,#5341,#5342,#5343,#5344,
#5345,#5346,#5347,#5348,#5349,#5350,#5351,#5352,#5353,#5354,#5355));
#5534=CLOSED_SHELL('',(#5356,#5357,#5358,#5359));
#5535=CLOSED_SHELL('',(#5360,#5361,#5362,#5363));
#5536=CLOSED_SHELL('',(#5364,#5365,#5366,#5367));
#5537=CLOSED_SHELL('',(#5368,#5369,#5370,#5371,#5372,#5373,#5374,#5375,
#5376,#5377,#5378,#5379,#5380,#5381,#5382,#5383));
#5538=CLOSED_SHELL('',(#5384,#5385,#5386,#5387,#5388,#5389,#5390,#5391,
#5392,#5393,#5394,#5395,#5396,#5397,#5398));
#5539=CLOSED_SHELL('',(#5399,#5400,#5401,#5402,#5403,#5404,#5405,#5406,
#5407,#5408));
#5540=CLOSED_SHELL('',(#5409,#5410,#5411,#5412,#5413,#5414,#5415,#5416,
#5417,#5418));
#5541=CLOSED_SHELL('',(#5419,#5420,#5421,#5422,#5423,#5424,#5425,#5426,
#5427));
#5542=CLOSED_SHELL('',(#5428,#5429,#5430,#5431,#5432,#5433,#5434,#5435));
#5543=CLOSED_SHELL('',(#5436,#5437,#5438,#5439));
#5544=CLOSED_SHELL('',(#5440,#5441,#5442,#5443,#5444,#5445,#5446,#5447,
#5448,#5449,#5450));
#5545=CLOSED_SHELL('',(#5451,#5452,#5453,#5454,#5455,#5456,#5457));
#5546=CLOSED_SHELL('',(#5458,#5459,#5460,#5461,#5462,#5463,#5464,#5465,
#5466,#5467,#5468,#5469,#5470,#5471,#5472,#5473,#5474,#5475,#5476,#5477,
#5478,#5479));
#5547=CLOSED_SHELL('',(#5480,#5481,#5482,#5483,#5484,#5485,#5486,#5487,
#5488,#5489));
#5548=CLOSED_SHELL('',(#5490,#5491,#5492,#5493));
#5549=CLOSED_SHELL('',(#5494,#5495,#5496,#5497,#5498,#5499));
#5550=CLOSED_SHELL('',(#5500,#5501,#5502,#5503,#5504,#5505,#5506,#5507));
#5551=CLOSED_SHELL('',(#5508,#5509,#5510,#5511,#5512,#5513,#5514,#5515));
#5552=DERIVED_UNIT_ELEMENT(#5616,1.);
#5553=DERIVED_UNIT_ELEMENT(#10097,-3.);
#5554=DERIVED_UNIT_ELEMENT(#5616,1.);
#5555=DERIVED_UNIT_ELEMENT(#10097,-3.);
#5556=DERIVED_UNIT_ELEMENT(#5616,1.);
#5557=DERIVED_UNIT_ELEMENT(#10097,-3.);
#5558=DERIVED_UNIT_ELEMENT(#5616,1.);
#5559=DERIVED_UNIT_ELEMENT(#10097,-3.);
#5560=DERIVED_UNIT_ELEMENT(#5616,1.);
#5561=DERIVED_UNIT_ELEMENT(#10097,-3.);
#5562=DERIVED_UNIT_ELEMENT(#5616,1.);
#5563=DERIVED_UNIT_ELEMENT(#10097,-3.);
#5564=DERIVED_UNIT_ELEMENT(#5616,1.);
#5565=DERIVED_UNIT_ELEMENT(#10097,-3.);
#5566=DERIVED_UNIT_ELEMENT(#5616,1.);
#5567=DERIVED_UNIT_ELEMENT(#10097,-3.);
#5568=DERIVED_UNIT_ELEMENT(#5616,1.);
#5569=DERIVED_UNIT_ELEMENT(#10097,-3.);
#5570=DERIVED_UNIT_ELEMENT(#5616,1.);
#5571=DERIVED_UNIT_ELEMENT(#10097,-3.);
#5572=DERIVED_UNIT_ELEMENT(#5616,1.);
#5573=DERIVED_UNIT_ELEMENT(#10097,-3.);
#5574=DERIVED_UNIT_ELEMENT(#5616,1.);
#5575=DERIVED_UNIT_ELEMENT(#10097,-3.);
#5576=DERIVED_UNIT_ELEMENT(#5616,1.);
#5577=DERIVED_UNIT_ELEMENT(#10097,-3.);
#5578=DERIVED_UNIT_ELEMENT(#5616,1.);
#5579=DERIVED_UNIT_ELEMENT(#10097,-3.);
#5580=DERIVED_UNIT_ELEMENT(#5616,1.);
#5581=DERIVED_UNIT_ELEMENT(#10097,-3.);
#5582=DERIVED_UNIT_ELEMENT(#5616,1.);
#5583=DERIVED_UNIT_ELEMENT(#10097,-3.);
#5584=DERIVED_UNIT_ELEMENT(#5616,1.);
#5585=DERIVED_UNIT_ELEMENT(#10097,-3.);
#5586=DERIVED_UNIT_ELEMENT(#5616,1.);
#5587=DERIVED_UNIT_ELEMENT(#10097,-3.);
#5588=DERIVED_UNIT_ELEMENT(#5616,1.);
#5589=DERIVED_UNIT_ELEMENT(#10097,-3.);
#5590=DERIVED_UNIT_ELEMENT(#5616,1.);
#5591=DERIVED_UNIT_ELEMENT(#10097,-3.);
#5592=DERIVED_UNIT_ELEMENT(#5616,1.);
#5593=DERIVED_UNIT_ELEMENT(#10097,-3.);
#5594=DERIVED_UNIT_ELEMENT(#5616,1.);
#5595=DERIVED_UNIT_ELEMENT(#10097,-3.);
#5596=DERIVED_UNIT_ELEMENT(#5616,1.);
#5597=DERIVED_UNIT_ELEMENT(#10097,-3.);
#5598=DERIVED_UNIT_ELEMENT(#5616,1.);
#5599=DERIVED_UNIT_ELEMENT(#10097,-3.);
#5600=DERIVED_UNIT_ELEMENT(#5616,1.);
#5601=DERIVED_UNIT_ELEMENT(#10097,-3.);
#5602=DERIVED_UNIT_ELEMENT(#5616,1.);
#5603=DERIVED_UNIT_ELEMENT(#10097,-3.);
#5604=DERIVED_UNIT_ELEMENT(#5616,1.);
#5605=DERIVED_UNIT_ELEMENT(#10097,-3.);
#5606=DERIVED_UNIT_ELEMENT(#5616,1.);
#5607=DERIVED_UNIT_ELEMENT(#10097,-3.);
#5608=DERIVED_UNIT_ELEMENT(#5616,1.);
#5609=DERIVED_UNIT_ELEMENT(#10097,-3.);
#5610=DERIVED_UNIT_ELEMENT(#5616,1.);
#5611=DERIVED_UNIT_ELEMENT(#10097,-3.);
#5612=DERIVED_UNIT_ELEMENT(#5616,1.);
#5613=DERIVED_UNIT_ELEMENT(#10097,-3.);
#5614=DERIVED_UNIT_ELEMENT(#5616,1.);
#5615=DERIVED_UNIT_ELEMENT(#10097,-3.);
#5616=(
MASS_UNIT()
NAMED_UNIT(*)
SI_UNIT(.KILO.,.GRAM.)
);
#5617=DERIVED_UNIT((#5552,#5553));
#5618=DERIVED_UNIT((#5554,#5555));
#5619=DERIVED_UNIT((#5556,#5557));
#5620=DERIVED_UNIT((#5558,#5559));
#5621=DERIVED_UNIT((#5560,#5561));
#5622=DERIVED_UNIT((#5562,#5563));
#5623=DERIVED_UNIT((#5564,#5565));
#5624=DERIVED_UNIT((#5566,#5567));
#5625=DERIVED_UNIT((#5568,#5569));
#5626=DERIVED_UNIT((#5570,#5571));
#5627=DERIVED_UNIT((#5572,#5573));
#5628=DERIVED_UNIT((#5574,#5575));
#5629=DERIVED_UNIT((#5576,#5577));
#5630=DERIVED_UNIT((#5578,#5579));
#5631=DERIVED_UNIT((#5580,#5581));
#5632=DERIVED_UNIT((#5582,#5583));
#5633=DERIVED_UNIT((#5584,#5585));
#5634=DERIVED_UNIT((#5586,#5587));
#5635=DERIVED_UNIT((#5588,#5589));
#5636=DERIVED_UNIT((#5590,#5591));
#5637=DERIVED_UNIT((#5592,#5593));
#5638=DERIVED_UNIT((#5594,#5595));
#5639=DERIVED_UNIT((#5596,#5597));
#5640=DERIVED_UNIT((#5598,#5599));
#5641=DERIVED_UNIT((#5600,#5601));
#5642=DERIVED_UNIT((#5602,#5603));
#5643=DERIVED_UNIT((#5604,#5605));
#5644=DERIVED_UNIT((#5606,#5607));
#5645=DERIVED_UNIT((#5608,#5609));
#5646=DERIVED_UNIT((#5610,#5611));
#5647=DERIVED_UNIT((#5612,#5613));
#5648=DERIVED_UNIT((#5614,#5615));
#5649=MEASURE_REPRESENTATION_ITEM('density measure',
POSITIVE_RATIO_MEASURE(7850.),#5617);
#5650=MEASURE_REPRESENTATION_ITEM('density measure',
POSITIVE_RATIO_MEASURE(7850.),#5618);
#5651=MEASURE_REPRESENTATION_ITEM('density measure',
POSITIVE_RATIO_MEASURE(7850.),#5619);
#5652=MEASURE_REPRESENTATION_ITEM('density measure',
POSITIVE_RATIO_MEASURE(7850.),#5620);
#5653=MEASURE_REPRESENTATION_ITEM('density measure',
POSITIVE_RATIO_MEASURE(7850.),#5621);
#5654=MEASURE_REPRESENTATION_ITEM('density measure',
POSITIVE_RATIO_MEASURE(7850.),#5622);
#5655=MEASURE_REPRESENTATION_ITEM('density measure',
POSITIVE_RATIO_MEASURE(7850.),#5623);
#5656=MEASURE_REPRESENTATION_ITEM('density measure',
POSITIVE_RATIO_MEASURE(7850.),#5624);
#5657=MEASURE_REPRESENTATION_ITEM('density measure',
POSITIVE_RATIO_MEASURE(7850.),#5625);
#5658=MEASURE_REPRESENTATION_ITEM('density measure',
POSITIVE_RATIO_MEASURE(7850.),#5626);
#5659=MEASURE_REPRESENTATION_ITEM('density measure',
POSITIVE_RATIO_MEASURE(7850.),#5627);
#5660=MEASURE_REPRESENTATION_ITEM('density measure',
POSITIVE_RATIO_MEASURE(7850.),#5628);
#5661=MEASURE_REPRESENTATION_ITEM('density measure',
POSITIVE_RATIO_MEASURE(7850.),#5629);
#5662=MEASURE_REPRESENTATION_ITEM('density measure',
POSITIVE_RATIO_MEASURE(7850.),#5630);
#5663=MEASURE_REPRESENTATION_ITEM('density measure',
POSITIVE_RATIO_MEASURE(7850.),#5631);
#5664=MEASURE_REPRESENTATION_ITEM('density measure',
POSITIVE_RATIO_MEASURE(7850.),#5632);
#5665=MEASURE_REPRESENTATION_ITEM('density measure',
POSITIVE_RATIO_MEASURE(7850.),#5633);
#5666=MEASURE_REPRESENTATION_ITEM('density measure',
POSITIVE_RATIO_MEASURE(7850.),#5634);
#5667=MEASURE_REPRESENTATION_ITEM('density measure',
POSITIVE_RATIO_MEASURE(7850.),#5635);
#5668=MEASURE_REPRESENTATION_ITEM('density measure',
POSITIVE_RATIO_MEASURE(7850.),#5636);
#5669=MEASURE_REPRESENTATION_ITEM('density measure',
POSITIVE_RATIO_MEASURE(7850.),#5637);
#5670=MEASURE_REPRESENTATION_ITEM('density measure',
POSITIVE_RATIO_MEASURE(7850.),#5638);
#5671=MEASURE_REPRESENTATION_ITEM('density measure',
POSITIVE_RATIO_MEASURE(7850.),#5639);
#5672=MEASURE_REPRESENTATION_ITEM('density measure',
POSITIVE_RATIO_MEASURE(7850.),#5640);
#5673=MEASURE_REPRESENTATION_ITEM('density measure',
POSITIVE_RATIO_MEASURE(7850.),#5641);
#5674=MEASURE_REPRESENTATION_ITEM('density measure',
POSITIVE_RATIO_MEASURE(7850.),#5642);
#5675=MEASURE_REPRESENTATION_ITEM('density measure',
POSITIVE_RATIO_MEASURE(7850.),#5643);
#5676=MEASURE_REPRESENTATION_ITEM('density measure',
POSITIVE_RATIO_MEASURE(7850.),#5644);
#5677=MEASURE_REPRESENTATION_ITEM('density measure',
POSITIVE_RATIO_MEASURE(7850.),#5645);
#5678=MEASURE_REPRESENTATION_ITEM('density measure',
POSITIVE_RATIO_MEASURE(7850.),#5646);
#5679=MEASURE_REPRESENTATION_ITEM('density measure',
POSITIVE_RATIO_MEASURE(7850.),#5647);
#5680=MEASURE_REPRESENTATION_ITEM('density measure',
POSITIVE_RATIO_MEASURE(7850.),#5648);
#5681=PROPERTY_DEFINITION_REPRESENTATION(#5841,#5745);
#5682=PROPERTY_DEFINITION_REPRESENTATION(#5842,#5746);
#5683=PROPERTY_DEFINITION_REPRESENTATION(#5843,#5747);
#5684=PROPERTY_DEFINITION_REPRESENTATION(#5844,#5748);
#5685=PROPERTY_DEFINITION_REPRESENTATION(#5845,#5749);
#5686=PROPERTY_DEFINITION_REPRESENTATION(#5846,#5750);
#5687=PROPERTY_DEFINITION_REPRESENTATION(#5847,#5751);
#5688=PROPERTY_DEFINITION_REPRESENTATION(#5848,#5752);
#5689=PROPERTY_DEFINITION_REPRESENTATION(#5849,#5753);
#5690=PROPERTY_DEFINITION_REPRESENTATION(#5850,#5754);
#5691=PROPERTY_DEFINITION_REPRESENTATION(#5851,#5755);
#5692=PROPERTY_DEFINITION_REPRESENTATION(#5852,#5756);
#5693=PROPERTY_DEFINITION_REPRESENTATION(#5853,#5757);
#5694=PROPERTY_DEFINITION_REPRESENTATION(#5854,#5758);
#5695=PROPERTY_DEFINITION_REPRESENTATION(#5855,#5759);
#5696=PROPERTY_DEFINITION_REPRESENTATION(#5856,#5760);
#5697=PROPERTY_DEFINITION_REPRESENTATION(#5857,#5761);
#5698=PROPERTY_DEFINITION_REPRESENTATION(#5858,#5762);
#5699=PROPERTY_DEFINITION_REPRESENTATION(#5859,#5763);
#5700=PROPERTY_DEFINITION_REPRESENTATION(#5860,#5764);
#5701=PROPERTY_DEFINITION_REPRESENTATION(#5861,#5765);
#5702=PROPERTY_DEFINITION_REPRESENTATION(#5862,#5766);
#5703=PROPERTY_DEFINITION_REPRESENTATION(#5863,#5767);
#5704=PROPERTY_DEFINITION_REPRESENTATION(#5864,#5768);
#5705=PROPERTY_DEFINITION_REPRESENTATION(#5865,#5769);
#5706=PROPERTY_DEFINITION_REPRESENTATION(#5866,#5770);
#5707=PROPERTY_DEFINITION_REPRESENTATION(#5867,#5771);
#5708=PROPERTY_DEFINITION_REPRESENTATION(#5868,#5772);
#5709=PROPERTY_DEFINITION_REPRESENTATION(#5869,#5773);
#5710=PROPERTY_DEFINITION_REPRESENTATION(#5870,#5774);
#5711=PROPERTY_DEFINITION_REPRESENTATION(#5871,#5775);
#5712=PROPERTY_DEFINITION_REPRESENTATION(#5872,#5776);
#5713=PROPERTY_DEFINITION_REPRESENTATION(#5873,#5777);
#5714=PROPERTY_DEFINITION_REPRESENTATION(#5874,#5778);
#5715=PROPERTY_DEFINITION_REPRESENTATION(#5875,#5779);
#5716=PROPERTY_DEFINITION_REPRESENTATION(#5876,#5780);
#5717=PROPERTY_DEFINITION_REPRESENTATION(#5877,#5781);
#5718=PROPERTY_DEFINITION_REPRESENTATION(#5878,#5782);
#5719=PROPERTY_DEFINITION_REPRESENTATION(#5879,#5783);
#5720=PROPERTY_DEFINITION_REPRESENTATION(#5880,#5784);
#5721=PROPERTY_DEFINITION_REPRESENTATION(#5881,#5785);
#5722=PROPERTY_DEFINITION_REPRESENTATION(#5882,#5786);
#5723=PROPERTY_DEFINITION_REPRESENTATION(#5883,#5787);
#5724=PROPERTY_DEFINITION_REPRESENTATION(#5884,#5788);
#5725=PROPERTY_DEFINITION_REPRESENTATION(#5885,#5789);
#5726=PROPERTY_DEFINITION_REPRESENTATION(#5886,#5790);
#5727=PROPERTY_DEFINITION_REPRESENTATION(#5887,#5791);
#5728=PROPERTY_DEFINITION_REPRESENTATION(#5888,#5792);
#5729=PROPERTY_DEFINITION_REPRESENTATION(#5889,#5793);
#5730=PROPERTY_DEFINITION_REPRESENTATION(#5890,#5794);
#5731=PROPERTY_DEFINITION_REPRESENTATION(#5891,#5795);
#5732=PROPERTY_DEFINITION_REPRESENTATION(#5892,#5796);
#5733=PROPERTY_DEFINITION_REPRESENTATION(#5893,#5797);
#5734=PROPERTY_DEFINITION_REPRESENTATION(#5894,#5798);
#5735=PROPERTY_DEFINITION_REPRESENTATION(#5895,#5799);
#5736=PROPERTY_DEFINITION_REPRESENTATION(#5896,#5800);
#5737=PROPERTY_DEFINITION_REPRESENTATION(#5897,#5801);
#5738=PROPERTY_DEFINITION_REPRESENTATION(#5898,#5802);
#5739=PROPERTY_DEFINITION_REPRESENTATION(#5899,#5803);
#5740=PROPERTY_DEFINITION_REPRESENTATION(#5900,#5804);
#5741=PROPERTY_DEFINITION_REPRESENTATION(#5901,#5805);
#5742=PROPERTY_DEFINITION_REPRESENTATION(#5902,#5806);
#5743=PROPERTY_DEFINITION_REPRESENTATION(#5903,#5807);
#5744=PROPERTY_DEFINITION_REPRESENTATION(#5904,#5808);
#5745=REPRESENTATION('material name',(#5809),#10062);
#5746=REPRESENTATION('density',(#5649),#10062);
#5747=REPRESENTATION('material name',(#5810),#10063);
#5748=REPRESENTATION('density',(#5650),#10063);
#5749=REPRESENTATION('material name',(#5811),#10064);
#5750=REPRESENTATION('density',(#5651),#10064);
#5751=REPRESENTATION('material name',(#5812),#10065);
#5752=REPRESENTATION('density',(#5652),#10065);
#5753=REPRESENTATION('material name',(#5813),#10066);
#5754=REPRESENTATION('density',(#5653),#10066);
#5755=REPRESENTATION('material name',(#5814),#10067);
#5756=REPRESENTATION('density',(#5654),#10067);
#5757=REPRESENTATION('material name',(#5815),#10068);
#5758=REPRESENTATION('density',(#5655),#10068);
#5759=REPRESENTATION('material name',(#5816),#10069);
#5760=REPRESENTATION('density',(#5656),#10069);
#5761=REPRESENTATION('material name',(#5817),#10070);
#5762=REPRESENTATION('density',(#5657),#10070);
#5763=REPRESENTATION('material name',(#5818),#10071);
#5764=REPRESENTATION('density',(#5658),#10071);
#5765=REPRESENTATION('material name',(#5819),#10072);
#5766=REPRESENTATION('density',(#5659),#10072);
#5767=REPRESENTATION('material name',(#5820),#10073);
#5768=REPRESENTATION('density',(#5660),#10073);
#5769=REPRESENTATION('material name',(#5821),#10074);
#5770=REPRESENTATION('density',(#5661),#10074);
#5771=REPRESENTATION('material name',(#5822),#10075);
#5772=REPRESENTATION('density',(#5662),#10075);
#5773=REPRESENTATION('material name',(#5823),#10076);
#5774=REPRESENTATION('density',(#5663),#10076);
#5775=REPRESENTATION('material name',(#5824),#10077);
#5776=REPRESENTATION('density',(#5664),#10077);
#5777=REPRESENTATION('material name',(#5825),#10078);
#5778=REPRESENTATION('density',(#5665),#10078);
#5779=REPRESENTATION('material name',(#5826),#10079);
#5780=REPRESENTATION('density',(#5666),#10079);
#5781=REPRESENTATION('material name',(#5827),#10080);
#5782=REPRESENTATION('density',(#5667),#10080);
#5783=REPRESENTATION('material name',(#5828),#10081);
#5784=REPRESENTATION('density',(#5668),#10081);
#5785=REPRESENTATION('material name',(#5829),#10082);
#5786=REPRESENTATION('density',(#5669),#10082);
#5787=REPRESENTATION('material name',(#5830),#10083);
#5788=REPRESENTATION('density',(#5670),#10083);
#5789=REPRESENTATION('material name',(#5831),#10084);
#5790=REPRESENTATION('density',(#5671),#10084);
#5791=REPRESENTATION('material name',(#5832),#10085);
#5792=REPRESENTATION('density',(#5672),#10085);
#5793=REPRESENTATION('material name',(#5833),#10086);
#5794=REPRESENTATION('density',(#5673),#10086);
#5795=REPRESENTATION('material name',(#5834),#10087);
#5796=REPRESENTATION('density',(#5674),#10087);
#5797=REPRESENTATION('material name',(#5835),#10089);
#5798=REPRESENTATION('density',(#5675),#10089);
#5799=REPRESENTATION('material name',(#5836),#10090);
#5800=REPRESENTATION('density',(#5676),#10090);
#5801=REPRESENTATION('material name',(#5837),#10091);
#5802=REPRESENTATION('density',(#5677),#10091);
#5803=REPRESENTATION('material name',(#5838),#10092);
#5804=REPRESENTATION('density',(#5678),#10092);
#5805=REPRESENTATION('material name',(#5839),#10093);
#5806=REPRESENTATION('density',(#5679),#10093);
#5807=REPRESENTATION('material name',(#5840),#10094);
#5808=REPRESENTATION('density',(#5680),#10094);
#5809=DESCRIPTIVE_REPRESENTATION_ITEM('Steel','Steel');
#5810=DESCRIPTIVE_REPRESENTATION_ITEM('Steel','Steel');
#5811=DESCRIPTIVE_REPRESENTATION_ITEM('Steel','Steel');
#5812=DESCRIPTIVE_REPRESENTATION_ITEM('Steel','Steel');
#5813=DESCRIPTIVE_REPRESENTATION_ITEM('Steel','Steel');
#5814=DESCRIPTIVE_REPRESENTATION_ITEM('Steel','Steel');
#5815=DESCRIPTIVE_REPRESENTATION_ITEM('Steel','Steel');
#5816=DESCRIPTIVE_REPRESENTATION_ITEM('Steel','Steel');
#5817=DESCRIPTIVE_REPRESENTATION_ITEM('Steel','Steel');
#5818=DESCRIPTIVE_REPRESENTATION_ITEM('Steel','Steel');
#5819=DESCRIPTIVE_REPRESENTATION_ITEM('Steel','Steel');
#5820=DESCRIPTIVE_REPRESENTATION_ITEM('Steel','Steel');
#5821=DESCRIPTIVE_REPRESENTATION_ITEM('Steel','Steel');
#5822=DESCRIPTIVE_REPRESENTATION_ITEM('Steel','Steel');
#5823=DESCRIPTIVE_REPRESENTATION_ITEM('Steel','Steel');
#5824=DESCRIPTIVE_REPRESENTATION_ITEM('Steel','Steel');
#5825=DESCRIPTIVE_REPRESENTATION_ITEM('Steel','Steel');
#5826=DESCRIPTIVE_REPRESENTATION_ITEM('Steel','Steel');
#5827=DESCRIPTIVE_REPRESENTATION_ITEM('Steel','Steel');
#5828=DESCRIPTIVE_REPRESENTATION_ITEM('Steel','Steel');
#5829=DESCRIPTIVE_REPRESENTATION_ITEM('Steel','Steel');
#5830=DESCRIPTIVE_REPRESENTATION_ITEM('Steel','Steel');
#5831=DESCRIPTIVE_REPRESENTATION_ITEM('Steel','Steel');
#5832=DESCRIPTIVE_REPRESENTATION_ITEM('Steel','Steel');
#5833=DESCRIPTIVE_REPRESENTATION_ITEM('Steel','Steel');
#5834=DESCRIPTIVE_REPRESENTATION_ITEM('Steel','Steel');
#5835=DESCRIPTIVE_REPRESENTATION_ITEM('Steel','Steel');
#5836=DESCRIPTIVE_REPRESENTATION_ITEM('Steel','Steel');
#5837=DESCRIPTIVE_REPRESENTATION_ITEM('Steel','Steel');
#5838=DESCRIPTIVE_REPRESENTATION_ITEM('Steel','Steel');
#5839=DESCRIPTIVE_REPRESENTATION_ITEM('Steel','Steel');
#5840=DESCRIPTIVE_REPRESENTATION_ITEM('Steel','Steel');
#5841=PROPERTY_DEFINITION('material property','material name',#10287);
#5842=PROPERTY_DEFINITION('material property','density of part',#10287);
#5843=PROPERTY_DEFINITION('material property','material name',#10288);
#5844=PROPERTY_DEFINITION('material property','density of part',#10288);
#5845=PROPERTY_DEFINITION('material property','material name',#10289);
#5846=PROPERTY_DEFINITION('material property','density of part',#10289);
#5847=PROPERTY_DEFINITION('material property','material name',#10290);
#5848=PROPERTY_DEFINITION('material property','density of part',#10290);
#5849=PROPERTY_DEFINITION('material property','material name',#10291);
#5850=PROPERTY_DEFINITION('material property','density of part',#10291);
#5851=PROPERTY_DEFINITION('material property','material name',#10292);
#5852=PROPERTY_DEFINITION('material property','density of part',#10292);
#5853=PROPERTY_DEFINITION('material property','material name',#10293);
#5854=PROPERTY_DEFINITION('material property','density of part',#10293);
#5855=PROPERTY_DEFINITION('material property','material name',#10294);
#5856=PROPERTY_DEFINITION('material property','density of part',#10294);
#5857=PROPERTY_DEFINITION('material property','material name',#10295);
#5858=PROPERTY_DEFINITION('material property','density of part',#10295);
#5859=PROPERTY_DEFINITION('material property','material name',#10296);
#5860=PROPERTY_DEFINITION('material property','density of part',#10296);
#5861=PROPERTY_DEFINITION('material property','material name',#10297);
#5862=PROPERTY_DEFINITION('material property','density of part',#10297);
#5863=PROPERTY_DEFINITION('material property','material name',#10298);
#5864=PROPERTY_DEFINITION('material property','density of part',#10298);
#5865=PROPERTY_DEFINITION('material property','material name',#10299);
#5866=PROPERTY_DEFINITION('material property','density of part',#10299);
#5867=PROPERTY_DEFINITION('material property','material name',#10300);
#5868=PROPERTY_DEFINITION('material property','density of part',#10300);
#5869=PROPERTY_DEFINITION('material property','material name',#10301);
#5870=PROPERTY_DEFINITION('material property','density of part',#10301);
#5871=PROPERTY_DEFINITION('material property','material name',#10302);
#5872=PROPERTY_DEFINITION('material property','density of part',#10302);
#5873=PROPERTY_DEFINITION('material property','material name',#10303);
#5874=PROPERTY_DEFINITION('material property','density of part',#10303);
#5875=PROPERTY_DEFINITION('material property','material name',#10304);
#5876=PROPERTY_DEFINITION('material property','density of part',#10304);
#5877=PROPERTY_DEFINITION('material property','material name',#10305);
#5878=PROPERTY_DEFINITION('material property','density of part',#10305);
#5879=PROPERTY_DEFINITION('material property','material name',#10306);
#5880=PROPERTY_DEFINITION('material property','density of part',#10306);
#5881=PROPERTY_DEFINITION('material property','material name',#10307);
#5882=PROPERTY_DEFINITION('material property','density of part',#10307);
#5883=PROPERTY_DEFINITION('material property','material name',#10308);
#5884=PROPERTY_DEFINITION('material property','density of part',#10308);
#5885=PROPERTY_DEFINITION('material property','material name',#10309);
#5886=PROPERTY_DEFINITION('material property','density of part',#10309);
#5887=PROPERTY_DEFINITION('material property','material name',#10310);
#5888=PROPERTY_DEFINITION('material property','density of part',#10310);
#5889=PROPERTY_DEFINITION('material property','material name',#10311);
#5890=PROPERTY_DEFINITION('material property','density of part',#10311);
#5891=PROPERTY_DEFINITION('material property','material name',#10312);
#5892=PROPERTY_DEFINITION('material property','density of part',#10312);
#5893=PROPERTY_DEFINITION('material property','material name',#10314);
#5894=PROPERTY_DEFINITION('material property','density of part',#10314);
#5895=PROPERTY_DEFINITION('material property','material name',#10315);
#5896=PROPERTY_DEFINITION('material property','density of part',#10315);
#5897=PROPERTY_DEFINITION('material property','material name',#10316);
#5898=PROPERTY_DEFINITION('material property','density of part',#10316);
#5899=PROPERTY_DEFINITION('material property','material name',#10317);
#5900=PROPERTY_DEFINITION('material property','density of part',#10317);
#5901=PROPERTY_DEFINITION('material property','material name',#10318);
#5902=PROPERTY_DEFINITION('material property','density of part',#10318);
#5903=PROPERTY_DEFINITION('material property','material name',#10319);
#5904=PROPERTY_DEFINITION('material property','density of part',#10319);
#5905=AXIS2_PLACEMENT_3D('',#8423,#6619,#6620);
#5906=AXIS2_PLACEMENT_3D('',#8424,#6621,#6622);
#5907=AXIS2_PLACEMENT_3D('',#8425,#6623,#6624);
#5908=AXIS2_PLACEMENT_3D('',#8426,#6625,#6626);
#5909=AXIS2_PLACEMENT_3D('',#8427,#6627,#6628);
#5910=AXIS2_PLACEMENT_3D('',#8429,#6629,#6630);
#5911=AXIS2_PLACEMENT_3D('',#8432,#6632,#6633);
#5912=AXIS2_PLACEMENT_3D('',#8433,#6634,#6635);
#5913=AXIS2_PLACEMENT_3D('',#8434,#6636,#6637);
#5914=AXIS2_PLACEMENT_3D('',#8436,#6638,#6639);
#5915=AXIS2_PLACEMENT_3D('',#8439,#6641,#6642);
#5916=AXIS2_PLACEMENT_3D('',#8440,#6643,#6644);
#5917=AXIS2_PLACEMENT_3D('',#8441,#6645,#6646);
#5918=AXIS2_PLACEMENT_3D('',#8443,#6647,#6648);
#5919=AXIS2_PLACEMENT_3D('',#8446,#6650,#6651);
#5920=AXIS2_PLACEMENT_3D('',#8447,#6652,#6653);
#5921=AXIS2_PLACEMENT_3D('',#8449,#6654,#6655);
#5922=AXIS2_PLACEMENT_3D('',#8452,#6657,#6658);
#5923=AXIS2_PLACEMENT_3D('',#8453,#6659,#6660);
#5924=AXIS2_PLACEMENT_3D('',#8455,#6661,#6662);
#5925=AXIS2_PLACEMENT_3D('',#8458,#6664,#6665);
#5926=AXIS2_PLACEMENT_3D('',#8459,#6666,#6667);
#5927=AXIS2_PLACEMENT_3D('',#8461,#6668,#6669);
#5928=AXIS2_PLACEMENT_3D('',#8464,#6671,#6672);
#5929=AXIS2_PLACEMENT_3D('',#8465,#6673,#6674);
#5930=AXIS2_PLACEMENT_3D('',#8470,#6676,#6677);
#5931=AXIS2_PLACEMENT_3D('',#8473,#6679,#6680);
#5932=AXIS2_PLACEMENT_3D('',#8474,#6681,#6682);
#5933=AXIS2_PLACEMENT_3D('',#8478,#6684,#6685);
#5934=AXIS2_PLACEMENT_3D('',#8480,#6687,#6688);
#5935=AXIS2_PLACEMENT_3D('',#8490,#6694,#6695);
#5936=AXIS2_PLACEMENT_3D('',#8492,#6696,#6697);
#5937=AXIS2_PLACEMENT_3D('',#8495,#6699,#6700);
#5938=AXIS2_PLACEMENT_3D('',#8496,#6701,#6702);
#5939=AXIS2_PLACEMENT_3D('',#8498,#6703,#6704);
#5940=AXIS2_PLACEMENT_3D('',#8501,#6706,#6707);
#5941=AXIS2_PLACEMENT_3D('',#8502,#6708,#6709);
#5942=AXIS2_PLACEMENT_3D('',#8504,#6710,#6711);
#5943=AXIS2_PLACEMENT_3D('',#8505,#6712,#6713);
#5944=AXIS2_PLACEMENT_3D('',#8506,#6714,#6715);
#5945=AXIS2_PLACEMENT_3D('',#8507,#6716,#6717);
#5946=AXIS2_PLACEMENT_3D('',#8508,#6718,#6719);
#5947=AXIS2_PLACEMENT_3D('',#8514,#6723,#6724);
#5948=AXIS2_PLACEMENT_3D('',#8518,#6727,#6728);
#5949=AXIS2_PLACEMENT_3D('',#8522,#6731,#6732);
#5950=AXIS2_PLACEMENT_3D('',#8524,#6734,#6735);
#5951=AXIS2_PLACEMENT_3D('',#8525,#6736,#6737);
#5952=AXIS2_PLACEMENT_3D('',#8526,#6738,#6739);
#5953=AXIS2_PLACEMENT_3D('',#8528,#6740,#6741);
#5954=AXIS2_PLACEMENT_3D('',#8531,#6743,#6744);
#5955=AXIS2_PLACEMENT_3D('',#8532,#6745,#6746);
#5956=AXIS2_PLACEMENT_3D('',#8533,#6747,#6748);
#5957=AXIS2_PLACEMENT_3D('',#8535,#6749,#6750);
#5958=AXIS2_PLACEMENT_3D('',#8538,#6752,#6753);
#5959=AXIS2_PLACEMENT_3D('',#8539,#6754,#6755);
#5960=AXIS2_PLACEMENT_3D('',#8540,#6756,#6757);
#5961=AXIS2_PLACEMENT_3D('',#8542,#6758,#6759);
#5962=AXIS2_PLACEMENT_3D('',#8545,#6761,#6762);
#5963=AXIS2_PLACEMENT_3D('',#8546,#6763,#6764);
#5964=AXIS2_PLACEMENT_3D('',#8548,#6765,#6766);
#5965=AXIS2_PLACEMENT_3D('',#8551,#6768,#6769);
#5966=AXIS2_PLACEMENT_3D('',#8552,#6770,#6771);
#5967=AXIS2_PLACEMENT_3D('',#8554,#6772,#6773);
#5968=AXIS2_PLACEMENT_3D('',#8557,#6775,#6776);
#5969=AXIS2_PLACEMENT_3D('',#8558,#6777,#6778);
#5970=AXIS2_PLACEMENT_3D('',#8560,#6779,#6780);
#5971=AXIS2_PLACEMENT_3D('',#8563,#6782,#6783);
#5972=AXIS2_PLACEMENT_3D('',#8564,#6784,#6785);
#5973=AXIS2_PLACEMENT_3D('',#8569,#6787,#6788);
#5974=AXIS2_PLACEMENT_3D('',#8572,#6790,#6791);
#5975=AXIS2_PLACEMENT_3D('',#8573,#6792,#6793);
#5976=AXIS2_PLACEMENT_3D('',#8577,#6795,#6796);
#5977=AXIS2_PLACEMENT_3D('',#8579,#6798,#6799);
#5978=AXIS2_PLACEMENT_3D('',#8589,#6805,#6806);
#5979=AXIS2_PLACEMENT_3D('',#8591,#6807,#6808);
#5980=AXIS2_PLACEMENT_3D('',#8594,#6810,#6811);
#5981=AXIS2_PLACEMENT_3D('',#8595,#6812,#6813);
#5982=AXIS2_PLACEMENT_3D('',#8597,#6814,#6815);
#5983=AXIS2_PLACEMENT_3D('',#8600,#6817,#6818);
#5984=AXIS2_PLACEMENT_3D('',#8601,#6819,#6820);
#5985=AXIS2_PLACEMENT_3D('',#8602,#6821,#6822);
#5986=AXIS2_PLACEMENT_3D('',#8604,#6823,#6824);
#5987=AXIS2_PLACEMENT_3D('',#8605,#6825,#6826);
#5988=AXIS2_PLACEMENT_3D('',#8606,#6827,#6828);
#5989=AXIS2_PLACEMENT_3D('',#8607,#6829,#6830);
#5990=AXIS2_PLACEMENT_3D('',#8613,#6834,#6835);
#5991=AXIS2_PLACEMENT_3D('',#8617,#6838,#6839);
#5992=AXIS2_PLACEMENT_3D('',#8621,#6842,#6843);
#5993=AXIS2_PLACEMENT_3D('',#8623,#6845,#6846);
#5994=AXIS2_PLACEMENT_3D('',#8624,#6847,#6848);
#5995=AXIS2_PLACEMENT_3D('',#8625,#6849,#6850);
#5996=AXIS2_PLACEMENT_3D('',#8627,#6851,#6852);
#5997=AXIS2_PLACEMENT_3D('',#8630,#6854,#6855);
#5998=AXIS2_PLACEMENT_3D('',#8631,#6856,#6857);
#5999=AXIS2_PLACEMENT_3D('',#8633,#6858,#6859);
#6000=AXIS2_PLACEMENT_3D('',#8636,#6861,#6862);
#6001=AXIS2_PLACEMENT_3D('',#8637,#6863,#6864);
#6002=AXIS2_PLACEMENT_3D('',#8639,#6865,#6866);
#6003=AXIS2_PLACEMENT_3D('',#8642,#6868,#6869);
#6004=AXIS2_PLACEMENT_3D('',#8643,#6870,#6871);
#6005=AXIS2_PLACEMENT_3D('',#8645,#6872,#6873);
#6006=AXIS2_PLACEMENT_3D('',#8648,#6875,#6876);
#6007=AXIS2_PLACEMENT_3D('',#8649,#6877,#6878);
#6008=AXIS2_PLACEMENT_3D('',#8658,#6883,#6884);
#6009=AXIS2_PLACEMENT_3D('',#8667,#6889,#6890);
#6010=AXIS2_PLACEMENT_3D('',#8673,#6894,#6895);
#6011=AXIS2_PLACEMENT_3D('',#8679,#6899,#6900);
#6012=AXIS2_PLACEMENT_3D('',#8680,#6901,#6902);
#6013=AXIS2_PLACEMENT_3D('',#8690,#6908,#6909);
#6014=AXIS2_PLACEMENT_3D('',#8694,#6912,#6913);
#6015=AXIS2_PLACEMENT_3D('',#8698,#6916,#6917);
#6016=AXIS2_PLACEMENT_3D('',#8699,#6918,#6919);
#6017=AXIS2_PLACEMENT_3D('',#8700,#6920,#6921);
#6018=AXIS2_PLACEMENT_3D('',#8704,#6924,#6925);
#6019=AXIS2_PLACEMENT_3D('',#8708,#6928,#6929);
#6020=AXIS2_PLACEMENT_3D('',#8710,#6931,#6932);
#6021=AXIS2_PLACEMENT_3D('',#8711,#6933,#6934);
#6022=AXIS2_PLACEMENT_3D('',#8712,#6935,#6936);
#6023=AXIS2_PLACEMENT_3D('',#8714,#6937,#6938);
#6024=AXIS2_PLACEMENT_3D('',#8716,#6939,#6940);
#6025=AXIS2_PLACEMENT_3D('',#8717,#6941,#6942);
#6026=AXIS2_PLACEMENT_3D('',#8719,#6943,#6944);
#6027=AXIS2_PLACEMENT_3D('',#8721,#6946,#6947);
#6028=AXIS2_PLACEMENT_3D('',#8723,#6948,#6949);
#6029=AXIS2_PLACEMENT_3D('',#8724,#6950,#6951);
#6030=AXIS2_PLACEMENT_3D('',#8727,#6953,#6954);
#6031=AXIS2_PLACEMENT_3D('',#8728,#6955,#6956);
#6032=AXIS2_PLACEMENT_3D('',#8731,#6958,#6959);
#6033=AXIS2_PLACEMENT_3D('',#8732,#6960,#6961);
#6034=AXIS2_PLACEMENT_3D('',#8733,#6962,#6963);
#6035=AXIS2_PLACEMENT_3D('',#8734,#6964,#6965);
#6036=AXIS2_PLACEMENT_3D('',#8736,#6966,#6967);
#6037=AXIS2_PLACEMENT_3D('',#8737,#6968,#6969);
#6038=AXIS2_PLACEMENT_3D('',#8738,#6970,#6971);
#6039=AXIS2_PLACEMENT_3D('',#8739,#6972,#6973);
#6040=AXIS2_PLACEMENT_3D('',#8741,#6974,#6975);
#6041=AXIS2_PLACEMENT_3D('',#8744,#6977,#6978);
#6042=AXIS2_PLACEMENT_3D('',#8745,#6979,#6980);
#6043=AXIS2_PLACEMENT_3D('',#8747,#6981,#6982);
#6044=AXIS2_PLACEMENT_3D('',#8748,#6983,#6984);
#6045=AXIS2_PLACEMENT_3D('',#8750,#6985,#6986);
#6046=AXIS2_PLACEMENT_3D('',#8752,#6988,#6989);
#6047=AXIS2_PLACEMENT_3D('',#8754,#6990,#6991);
#6048=AXIS2_PLACEMENT_3D('',#8757,#6993,#6994);
#6049=AXIS2_PLACEMENT_3D('',#8758,#6995,#6996);
#6050=AXIS2_PLACEMENT_3D('',#8759,#6997,#6998);
#6051=AXIS2_PLACEMENT_3D('',#8760,#6999,#7000);
#6052=AXIS2_PLACEMENT_3D('',#8761,#7001,#7002);
#6053=AXIS2_PLACEMENT_3D('',#8763,#7003,#7004);
#6054=AXIS2_PLACEMENT_3D('',#8766,#7006,#7007);
#6055=AXIS2_PLACEMENT_3D('',#8767,#7008,#7009);
#6056=AXIS2_PLACEMENT_3D('',#8768,#7010,#7011);
#6057=AXIS2_PLACEMENT_3D('',#8770,#7012,#7013);
#6058=AXIS2_PLACEMENT_3D('',#8773,#7015,#7016);
#6059=AXIS2_PLACEMENT_3D('',#8774,#7017,#7018);
#6060=AXIS2_PLACEMENT_3D('',#8775,#7019,#7020);
#6061=AXIS2_PLACEMENT_3D('',#8777,#7021,#7022);
#6062=AXIS2_PLACEMENT_3D('',#8780,#7024,#7025);
#6063=AXIS2_PLACEMENT_3D('',#8781,#7026,#7027);
#6064=AXIS2_PLACEMENT_3D('',#8783,#7028,#7029);
#6065=AXIS2_PLACEMENT_3D('',#8786,#7031,#7032);
#6066=AXIS2_PLACEMENT_3D('',#8787,#7033,#7034);
#6067=AXIS2_PLACEMENT_3D('',#8789,#7035,#7036);
#6068=AXIS2_PLACEMENT_3D('',#8792,#7038,#7039);
#6069=AXIS2_PLACEMENT_3D('',#8793,#7040,#7041);
#6070=AXIS2_PLACEMENT_3D('',#8795,#7042,#7043);
#6071=AXIS2_PLACEMENT_3D('',#8798,#7045,#7046);
#6072=AXIS2_PLACEMENT_3D('',#8799,#7047,#7048);
#6073=AXIS2_PLACEMENT_3D('',#8801,#7049,#7050);
#6074=AXIS2_PLACEMENT_3D('',#8804,#7052,#7053);
#6075=AXIS2_PLACEMENT_3D('',#8805,#7054,#7055);
#6076=AXIS2_PLACEMENT_3D('',#8814,#7060,#7061);
#6077=AXIS2_PLACEMENT_3D('',#8820,#7065,#7066);
#6078=AXIS2_PLACEMENT_3D('',#8826,#7070,#7071);
#6079=AXIS2_PLACEMENT_3D('',#8829,#7074,#7075);
#6080=AXIS2_PLACEMENT_3D('',#8830,#7076,#7077);
#6081=AXIS2_PLACEMENT_3D('',#8831,#7078,#7079);
#6082=AXIS2_PLACEMENT_3D('',#8832,#7080,#7081);
#6083=AXIS2_PLACEMENT_3D('',#8834,#7082,#7083);
#6084=AXIS2_PLACEMENT_3D('',#8836,#7084,#7085);
#6085=AXIS2_PLACEMENT_3D('',#8837,#7086,#7087);
#6086=AXIS2_PLACEMENT_3D('',#8840,#7089,#7090);
#6087=AXIS2_PLACEMENT_3D('',#8841,#7091,#7092);
#6088=AXIS2_PLACEMENT_3D('',#8843,#7093,#7094);
#6089=AXIS2_PLACEMENT_3D('',#8846,#7096,#7097);
#6090=AXIS2_PLACEMENT_3D('',#8847,#7098,#7099);
#6091=AXIS2_PLACEMENT_3D('',#8848,#7100,#7101);
#6092=AXIS2_PLACEMENT_3D('',#8849,#7102,#7103);
#6093=AXIS2_PLACEMENT_3D('',#8850,#7104,#7105);
#6094=AXIS2_PLACEMENT_3D('',#8859,#7110,#7111);
#6095=AXIS2_PLACEMENT_3D('',#8865,#7115,#7116);
#6096=AXIS2_PLACEMENT_3D('',#8871,#7120,#7121);
#6097=AXIS2_PLACEMENT_3D('',#8877,#7125,#7126);
#6098=AXIS2_PLACEMENT_3D('',#8883,#7130,#7131);
#6099=AXIS2_PLACEMENT_3D('',#8886,#7134,#7135);
#6100=AXIS2_PLACEMENT_3D('',#8887,#7136,#7137);
#6101=AXIS2_PLACEMENT_3D('',#8888,#7138,#7139);
#6102=AXIS2_PLACEMENT_3D('',#8890,#7140,#7141);
#6103=AXIS2_PLACEMENT_3D('',#8892,#7142,#7143);
#6104=AXIS2_PLACEMENT_3D('',#8893,#7144,#7145);
#6105=AXIS2_PLACEMENT_3D('',#8896,#7147,#7148);
#6106=AXIS2_PLACEMENT_3D('',#8897,#7149,#7150);
#6107=AXIS2_PLACEMENT_3D('',#8898,#7151,#7152);
#6108=AXIS2_PLACEMENT_3D('',#8900,#7153,#7154);
#6109=AXIS2_PLACEMENT_3D('',#8901,#7155,#7156);
#6110=AXIS2_PLACEMENT_3D('',#8903,#7157,#7158);
#6111=AXIS2_PLACEMENT_3D('',#8905,#7160,#7161);
#6112=AXIS2_PLACEMENT_3D('',#8907,#7162,#7163);
#6113=AXIS2_PLACEMENT_3D('',#8909,#7165,#7166);
#6114=AXIS2_PLACEMENT_3D('',#8911,#7167,#7168);
#6115=AXIS2_PLACEMENT_3D('',#8913,#7170,#7171);
#6116=AXIS2_PLACEMENT_3D('',#8915,#7172,#7173);
#6117=AXIS2_PLACEMENT_3D('',#8916,#7174,#7175);
#6118=AXIS2_PLACEMENT_3D('',#8918,#7176,#7177);
#6119=AXIS2_PLACEMENT_3D('',#8920,#7179,#7180);
#6120=AXIS2_PLACEMENT_3D('',#8922,#7182,#7183);
#6121=AXIS2_PLACEMENT_3D('',#8923,#7184,#7185);
#6122=AXIS2_PLACEMENT_3D('',#8925,#7186,#7187);
#6123=AXIS2_PLACEMENT_3D('',#8928,#7189,#7190);
#6124=AXIS2_PLACEMENT_3D('',#8929,#7191,#7192);
#6125=AXIS2_PLACEMENT_3D('',#8932,#7194,#7195);
#6126=AXIS2_PLACEMENT_3D('',#8933,#7196,#7197);
#6127=AXIS2_PLACEMENT_3D('',#8935,#7198,#7199);
#6128=AXIS2_PLACEMENT_3D('',#8936,#7200,#7201);
#6129=AXIS2_PLACEMENT_3D('',#8939,#7203,#7204);
#6130=AXIS2_PLACEMENT_3D('',#8940,#7205,#7206);
#6131=AXIS2_PLACEMENT_3D('',#8941,#7207,#7208);
#6132=AXIS2_PLACEMENT_3D('',#8942,#7209,#7210);
#6133=AXIS2_PLACEMENT_3D('',#8954,#7212,#7213);
#6134=AXIS2_PLACEMENT_3D('',#8970,#7214,#7215);
#6135=AXIS2_PLACEMENT_3D('',#8972,#7216,#7217);
#6136=AXIS2_PLACEMENT_3D('',#8998,#7219,#7220);
#6137=AXIS2_PLACEMENT_3D('',#9001,#7223,#7224);
#6138=AXIS2_PLACEMENT_3D('',#9003,#7226,#7227);
#6139=AXIS2_PLACEMENT_3D('',#9005,#7229,#7230);
#6140=AXIS2_PLACEMENT_3D('',#9007,#7231,#7232);
#6141=AXIS2_PLACEMENT_3D('',#9010,#7234,#7235);
#6142=AXIS2_PLACEMENT_3D('',#9011,#7236,#7237);
#6143=AXIS2_PLACEMENT_3D('',#9013,#7239,#7240);
#6144=AXIS2_PLACEMENT_3D('',#9015,#7242,#7243);
#6145=AXIS2_PLACEMENT_3D('',#9016,#7244,#7245);
#6146=AXIS2_PLACEMENT_3D('',#9017,#7246,#7247);
#6147=AXIS2_PLACEMENT_3D('',#9018,#7248,#7249);
#6148=AXIS2_PLACEMENT_3D('',#9019,#7250,#7251);
#6149=AXIS2_PLACEMENT_3D('',#9021,#7252,#7253);
#6150=AXIS2_PLACEMENT_3D('',#9024,#7255,#7256);
#6151=AXIS2_PLACEMENT_3D('',#9025,#7257,#7258);
#6152=AXIS2_PLACEMENT_3D('',#9027,#7259,#7260);
#6153=AXIS2_PLACEMENT_3D('',#9030,#7262,#7263);
#6154=AXIS2_PLACEMENT_3D('',#9031,#7264,#7265);
#6155=AXIS2_PLACEMENT_3D('',#9032,#7266,#7267);
#6156=AXIS2_PLACEMENT_3D('',#9033,#7268,#7269);
#6157=AXIS2_PLACEMENT_3D('',#9034,#7270,#7271);
#6158=AXIS2_PLACEMENT_3D('',#9036,#7272,#7273);
#6159=AXIS2_PLACEMENT_3D('',#9037,#7274,#7275);
#6160=AXIS2_PLACEMENT_3D('',#9039,#7276,#7277);
#6161=AXIS2_PLACEMENT_3D('',#9041,#7279,#7280);
#6162=AXIS2_PLACEMENT_3D('',#9043,#7281,#7282);
#6163=AXIS2_PLACEMENT_3D('',#9045,#7284,#7285);
#6164=AXIS2_PLACEMENT_3D('',#9047,#7286,#7287);
#6165=AXIS2_PLACEMENT_3D('',#9049,#7289,#7290);
#6166=AXIS2_PLACEMENT_3D('',#9051,#7291,#7292);
#6167=AXIS2_PLACEMENT_3D('',#9052,#7293,#7294);
#6168=AXIS2_PLACEMENT_3D('',#9054,#7295,#7296);
#6169=AXIS2_PLACEMENT_3D('',#9056,#7298,#7299);
#6170=AXIS2_PLACEMENT_3D('',#9058,#7300,#7301);
#6171=AXIS2_PLACEMENT_3D('',#9060,#7303,#7304);
#6172=AXIS2_PLACEMENT_3D('',#9062,#7305,#7306);
#6173=AXIS2_PLACEMENT_3D('',#9064,#7308,#7309);
#6174=AXIS2_PLACEMENT_3D('',#9065,#7310,#7311);
#6175=AXIS2_PLACEMENT_3D('',#9074,#7316,#7317);
#6176=AXIS2_PLACEMENT_3D('',#9080,#7321,#7322);
#6177=AXIS2_PLACEMENT_3D('',#9086,#7326,#7327);
#6178=AXIS2_PLACEMENT_3D('',#9092,#7331,#7332);
#6179=AXIS2_PLACEMENT_3D('',#9098,#7336,#7337);
#6180=AXIS2_PLACEMENT_3D('',#9101,#7340,#7341);
#6181=AXIS2_PLACEMENT_3D('',#9102,#7342,#7343);
#6182=AXIS2_PLACEMENT_3D('',#9103,#7344,#7345);
#6183=AXIS2_PLACEMENT_3D('',#9104,#7346,#7347);
#6184=AXIS2_PLACEMENT_3D('',#9106,#7348,#7349);
#6185=AXIS2_PLACEMENT_3D('',#9109,#7351,#7352);
#6186=AXIS2_PLACEMENT_3D('',#9110,#7353,#7354);
#6187=AXIS2_PLACEMENT_3D('',#9111,#7355,#7356);
#6188=AXIS2_PLACEMENT_3D('',#9112,#7357,#7358);
#6189=AXIS2_PLACEMENT_3D('',#9113,#7359,#7360);
#6190=AXIS2_PLACEMENT_3D('',#9114,#7361,#7362);
#6191=AXIS2_PLACEMENT_3D('',#9115,#7363,#7364);
#6192=AXIS2_PLACEMENT_3D('',#9116,#7365,#7366);
#6193=AXIS2_PLACEMENT_3D('',#9117,#7367,#7368);
#6194=AXIS2_PLACEMENT_3D('',#9118,#7369,#7370);
#6195=AXIS2_PLACEMENT_3D('',#9119,#7371,#7372);
#6196=AXIS2_PLACEMENT_3D('',#9120,#7373,#7374);
#6197=AXIS2_PLACEMENT_3D('',#9121,#7375,#7376);
#6198=AXIS2_PLACEMENT_3D('',#9122,#7377,#7378);
#6199=AXIS2_PLACEMENT_3D('',#9123,#7379,#7380);
#6200=AXIS2_PLACEMENT_3D('',#9124,#7381,#7382);
#6201=AXIS2_PLACEMENT_3D('',#9125,#7383,#7384);
#6202=AXIS2_PLACEMENT_3D('',#9126,#7385,#7386);
#6203=AXIS2_PLACEMENT_3D('',#9127,#7387,#7388);
#6204=AXIS2_PLACEMENT_3D('',#9128,#7389,#7390);
#6205=AXIS2_PLACEMENT_3D('',#9129,#7391,#7392);
#6206=AXIS2_PLACEMENT_3D('',#9130,#7393,#7394);
#6207=AXIS2_PLACEMENT_3D('',#9131,#7395,#7396);
#6208=AXIS2_PLACEMENT_3D('',#9132,#7397,#7398);
#6209=AXIS2_PLACEMENT_3D('',#9133,#7399,#7400);
#6210=AXIS2_PLACEMENT_3D('',#9134,#7401,#7402);
#6211=AXIS2_PLACEMENT_3D('',#9135,#7403,#7404);
#6212=AXIS2_PLACEMENT_3D('',#9136,#7405,#7406);
#6213=AXIS2_PLACEMENT_3D('',#9137,#7407,#7408);
#6214=AXIS2_PLACEMENT_3D('',#9138,#7409,#7410);
#6215=AXIS2_PLACEMENT_3D('',#9139,#7411,#7412);
#6216=AXIS2_PLACEMENT_3D('',#9140,#7413,#7414);
#6217=AXIS2_PLACEMENT_3D('',#9141,#7415,#7416);
#6218=AXIS2_PLACEMENT_3D('',#9142,#7417,#7418);
#6219=AXIS2_PLACEMENT_3D('',#9143,#7419,#7420);
#6220=AXIS2_PLACEMENT_3D('',#9144,#7421,#7422);
#6221=AXIS2_PLACEMENT_3D('',#9145,#7423,#7424);
#6222=AXIS2_PLACEMENT_3D('',#9146,#7425,#7426);
#6223=AXIS2_PLACEMENT_3D('',#9147,#7427,#7428);
#6224=AXIS2_PLACEMENT_3D('',#9148,#7429,#7430);
#6225=AXIS2_PLACEMENT_3D('',#9150,#7431,#7432);
#6226=AXIS2_PLACEMENT_3D('',#9153,#7434,#7435);
#6227=AXIS2_PLACEMENT_3D('',#9154,#7436,#7437);
#6228=AXIS2_PLACEMENT_3D('',#9156,#7438,#7439);
#6229=AXIS2_PLACEMENT_3D('',#9159,#7441,#7442);
#6230=AXIS2_PLACEMENT_3D('',#9160,#7443,#7444);
#6231=AXIS2_PLACEMENT_3D('',#9161,#7445,#7446);
#6232=AXIS2_PLACEMENT_3D('',#9162,#7447,#7448);
#6233=AXIS2_PLACEMENT_3D('',#9163,#7449,#7450);
#6234=AXIS2_PLACEMENT_3D('',#9168,#7452,#7453);
#6235=AXIS2_PLACEMENT_3D('',#9171,#7455,#7456);
#6236=AXIS2_PLACEMENT_3D('',#9172,#7457,#7458);
#6237=AXIS2_PLACEMENT_3D('',#9174,#7459,#7460);
#6238=AXIS2_PLACEMENT_3D('',#9177,#7462,#7463);
#6239=AXIS2_PLACEMENT_3D('',#9179,#7464,#7465);
#6240=AXIS2_PLACEMENT_3D('',#9181,#7466,#7467);
#6241=AXIS2_PLACEMENT_3D('',#9182,#7468,#7469);
#6242=AXIS2_PLACEMENT_3D('',#9183,#7470,#7471);
#6243=AXIS2_PLACEMENT_3D('',#9187,#7473,#7474);
#6244=AXIS2_PLACEMENT_3D('',#9189,#7476,#7477);
#6245=AXIS2_PLACEMENT_3D('',#9191,#7478,#7479);
#6246=AXIS2_PLACEMENT_3D('',#9194,#7481,#7482);
#6247=AXIS2_PLACEMENT_3D('',#9195,#7483,#7484);
#6248=AXIS2_PLACEMENT_3D('',#9196,#7485,#7486);
#6249=AXIS2_PLACEMENT_3D('',#9198,#7487,#7488);
#6250=AXIS2_PLACEMENT_3D('',#9199,#7489,#7490);
#6251=AXIS2_PLACEMENT_3D('',#9200,#7491,#7492);
#6252=AXIS2_PLACEMENT_3D('',#9201,#7493,#7494);
#6253=AXIS2_PLACEMENT_3D('',#9202,#7495,#7496);
#6254=AXIS2_PLACEMENT_3D('',#9204,#7497,#7498);
#6255=AXIS2_PLACEMENT_3D('',#9205,#7499,#7500);
#6256=AXIS2_PLACEMENT_3D('',#9206,#7501,#7502);
#6257=AXIS2_PLACEMENT_3D('',#9207,#7503,#7504);
#6258=AXIS2_PLACEMENT_3D('',#9209,#7505,#7506);
#6259=AXIS2_PLACEMENT_3D('',#9210,#7507,#7508);
#6260=AXIS2_PLACEMENT_3D('',#9211,#7509,#7510);
#6261=AXIS2_PLACEMENT_3D('',#9213,#7511,#7512);
#6262=AXIS2_PLACEMENT_3D('',#9215,#7514,#7515);
#6263=AXIS2_PLACEMENT_3D('',#9217,#7516,#7517);
#6264=AXIS2_PLACEMENT_3D('',#9220,#7519,#7520);
#6265=AXIS2_PLACEMENT_3D('',#9222,#7521,#7522);
#6266=AXIS2_PLACEMENT_3D('',#9225,#7524,#7525);
#6267=AXIS2_PLACEMENT_3D('',#9226,#7526,#7527);
#6268=AXIS2_PLACEMENT_3D('',#9227,#7528,#7529);
#6269=AXIS2_PLACEMENT_3D('',#9228,#7530,#7531);
#6270=AXIS2_PLACEMENT_3D('',#9229,#7532,#7533);
#6271=AXIS2_PLACEMENT_3D('',#9230,#7534,#7535);
#6272=AXIS2_PLACEMENT_3D('',#9231,#7536,#7537);
#6273=AXIS2_PLACEMENT_3D('',#9232,#7538,#7539);
#6274=AXIS2_PLACEMENT_3D('',#9235,#7540,#7541);
#6275=AXIS2_PLACEMENT_3D('',#9237,#7542,#7543);
#6276=AXIS2_PLACEMENT_3D('',#9240,#7545,#7546);
#6277=AXIS2_PLACEMENT_3D('',#9241,#7547,#7548);
#6278=AXIS2_PLACEMENT_3D('',#9242,#7549,#7550);
#6279=AXIS2_PLACEMENT_3D('',#9243,#7551,#7552);
#6280=AXIS2_PLACEMENT_3D('',#9245,#7553,#7554);
#6281=AXIS2_PLACEMENT_3D('',#9249,#7557,#7558);
#6282=AXIS2_PLACEMENT_3D('',#9250,#7559,#7560);
#6283=AXIS2_PLACEMENT_3D('',#9251,#7561,#7562);
#6284=AXIS2_PLACEMENT_3D('',#9252,#7563,#7564);
#6285=AXIS2_PLACEMENT_3D('',#9253,#7565,#7566);
#6286=AXIS2_PLACEMENT_3D('',#9255,#7567,#7568);
#6287=AXIS2_PLACEMENT_3D('',#9258,#7570,#7571);
#6288=AXIS2_PLACEMENT_3D('',#9259,#7572,#7573);
#6289=AXIS2_PLACEMENT_3D('',#9261,#7574,#7575);
#6290=AXIS2_PLACEMENT_3D('',#9264,#7577,#7578);
#6291=AXIS2_PLACEMENT_3D('',#9265,#7579,#7580);
#6292=AXIS2_PLACEMENT_3D('',#9266,#7581,#7582);
#6293=AXIS2_PLACEMENT_3D('',#9267,#7583,#7584);
#6294=AXIS2_PLACEMENT_3D('',#9268,#7585,#7586);
#6295=AXIS2_PLACEMENT_3D('',#9270,#7587,#7588);
#6296=AXIS2_PLACEMENT_3D('',#9273,#7590,#7591);
#6297=AXIS2_PLACEMENT_3D('',#9274,#7592,#7593);
#6298=AXIS2_PLACEMENT_3D('',#9276,#7594,#7595);
#6299=AXIS2_PLACEMENT_3D('',#9279,#7597,#7598);
#6300=AXIS2_PLACEMENT_3D('',#9280,#7599,#7600);
#6301=AXIS2_PLACEMENT_3D('',#9281,#7601,#7602);
#6302=AXIS2_PLACEMENT_3D('',#9282,#7603,#7604);
#6303=AXIS2_PLACEMENT_3D('',#9283,#7605,#7606);
#6304=AXIS2_PLACEMENT_3D('',#9285,#7607,#7608);
#6305=AXIS2_PLACEMENT_3D('',#9288,#7610,#7611);
#6306=AXIS2_PLACEMENT_3D('',#9289,#7612,#7613);
#6307=AXIS2_PLACEMENT_3D('',#9291,#7614,#7615);
#6308=AXIS2_PLACEMENT_3D('',#9294,#7617,#7618);
#6309=AXIS2_PLACEMENT_3D('',#9295,#7619,#7620);
#6310=AXIS2_PLACEMENT_3D('',#9296,#7621,#7622);
#6311=AXIS2_PLACEMENT_3D('',#9297,#7623,#7624);
#6312=AXIS2_PLACEMENT_3D('',#9298,#7625,#7626);
#6313=AXIS2_PLACEMENT_3D('',#9301,#7627,#7628);
#6314=AXIS2_PLACEMENT_3D('',#9303,#7629,#7630);
#6315=AXIS2_PLACEMENT_3D('',#9306,#7632,#7633);
#6316=AXIS2_PLACEMENT_3D('',#9307,#7634,#7635);
#6317=AXIS2_PLACEMENT_3D('',#9308,#7636,#7637);
#6318=AXIS2_PLACEMENT_3D('',#9311,#7638,#7639);
#6319=AXIS2_PLACEMENT_3D('',#9313,#7640,#7641);
#6320=AXIS2_PLACEMENT_3D('',#9314,#7642,#7643);
#6321=AXIS2_PLACEMENT_3D('',#9315,#7644,#7645);
#6322=AXIS2_PLACEMENT_3D('',#9318,#7647,#7648);
#6323=AXIS2_PLACEMENT_3D('',#9319,#7649,#7650);
#6324=AXIS2_PLACEMENT_3D('',#9321,#7651,#7652);
#6325=AXIS2_PLACEMENT_3D('',#9322,#7653,#7654);
#6326=AXIS2_PLACEMENT_3D('',#9324,#7655,#7656);
#6327=AXIS2_PLACEMENT_3D('',#9326,#7658,#7659);
#6328=AXIS2_PLACEMENT_3D('',#9328,#7660,#7661);
#6329=AXIS2_PLACEMENT_3D('',#9331,#7663,#7664);
#6330=AXIS2_PLACEMENT_3D('',#9332,#7665,#7666);
#6331=AXIS2_PLACEMENT_3D('',#9333,#7667,#7668);
#6332=AXIS2_PLACEMENT_3D('',#9336,#7669,#7670);
#6333=AXIS2_PLACEMENT_3D('',#9338,#7671,#7672);
#6334=AXIS2_PLACEMENT_3D('',#9340,#7673,#7674);
#6335=AXIS2_PLACEMENT_3D('',#9341,#7675,#7676);
#6336=AXIS2_PLACEMENT_3D('',#9342,#7677,#7678);
#6337=AXIS2_PLACEMENT_3D('',#9343,#7679,#7680);
#6338=AXIS2_PLACEMENT_3D('',#9346,#7682,#7683);
#6339=AXIS2_PLACEMENT_3D('',#9347,#7684,#7685);
#6340=AXIS2_PLACEMENT_3D('',#9349,#7686,#7687);
#6341=AXIS2_PLACEMENT_3D('',#9350,#7688,#7689);
#6342=AXIS2_PLACEMENT_3D('',#9352,#7690,#7691);
#6343=AXIS2_PLACEMENT_3D('',#9354,#7693,#7694);
#6344=AXIS2_PLACEMENT_3D('',#9355,#7695,#7696);
#6345=AXIS2_PLACEMENT_3D('',#9357,#7697,#7698);
#6346=AXIS2_PLACEMENT_3D('',#9359,#7699,#7700);
#6347=AXIS2_PLACEMENT_3D('',#9360,#7701,#7702);
#6348=AXIS2_PLACEMENT_3D('',#9362,#7703,#7704);
#6349=AXIS2_PLACEMENT_3D('',#9364,#7706,#7707);
#6350=AXIS2_PLACEMENT_3D('',#9365,#7708,#7709);
#6351=AXIS2_PLACEMENT_3D('',#9367,#7711,#7712);
#6352=AXIS2_PLACEMENT_3D('',#9368,#7713,#7714);
#6353=AXIS2_PLACEMENT_3D('',#9382,#7721,#7722);
#6354=AXIS2_PLACEMENT_3D('',#9383,#7723,#7724);
#6355=AXIS2_PLACEMENT_3D('',#9397,#7731,#7732);
#6356=AXIS2_PLACEMENT_3D('',#9398,#7733,#7734);
#6357=AXIS2_PLACEMENT_3D('',#9401,#7737,#7738);
#6358=AXIS2_PLACEMENT_3D('',#9403,#7740,#7741);
#6359=AXIS2_PLACEMENT_3D('',#9405,#7743,#7744);
#6360=AXIS2_PLACEMENT_3D('',#9407,#7746,#7747);
#6361=AXIS2_PLACEMENT_3D('',#9409,#7749,#7750);
#6362=AXIS2_PLACEMENT_3D('',#9410,#7751,#7752);
#6363=AXIS2_PLACEMENT_3D('',#9413,#7754,#7755);
#6364=AXIS2_PLACEMENT_3D('',#9414,#7756,#7757);
#6365=AXIS2_PLACEMENT_3D('',#9416,#7758,#7759);
#6366=AXIS2_PLACEMENT_3D('',#9418,#7760,#7761);
#6367=AXIS2_PLACEMENT_3D('',#9419,#7762,#7763);
#6368=AXIS2_PLACEMENT_3D('',#9421,#7765,#7766);
#6369=AXIS2_PLACEMENT_3D('',#9423,#7767,#7768);
#6370=AXIS2_PLACEMENT_3D('',#9425,#7770,#7771);
#6371=AXIS2_PLACEMENT_3D('',#9427,#7772,#7773);
#6372=AXIS2_PLACEMENT_3D('',#9429,#7775,#7776);
#6373=AXIS2_PLACEMENT_3D('',#9431,#7777,#7778);
#6374=AXIS2_PLACEMENT_3D('',#9432,#7779,#7780);
#6375=AXIS2_PLACEMENT_3D('',#9434,#7782,#7783);
#6376=AXIS2_PLACEMENT_3D('',#9435,#7784,#7785);
#6377=AXIS2_PLACEMENT_3D('',#9437,#7786,#7787);
#6378=AXIS2_PLACEMENT_3D('',#9440,#7789,#7790);
#6379=AXIS2_PLACEMENT_3D('',#9441,#7791,#7792);
#6380=AXIS2_PLACEMENT_3D('',#9443,#7793,#7794);
#6381=AXIS2_PLACEMENT_3D('',#9446,#7796,#7797);
#6382=AXIS2_PLACEMENT_3D('',#9447,#7798,#7799);
#6383=AXIS2_PLACEMENT_3D('',#9449,#7800,#7801);
#6384=AXIS2_PLACEMENT_3D('',#9452,#7803,#7804);
#6385=AXIS2_PLACEMENT_3D('',#9453,#7805,#7806);
#6386=AXIS2_PLACEMENT_3D('',#9455,#7807,#7808);
#6387=AXIS2_PLACEMENT_3D('',#9458,#7810,#7811);
#6388=AXIS2_PLACEMENT_3D('',#9459,#7812,#7813);
#6389=AXIS2_PLACEMENT_3D('',#9461,#7814,#7815);
#6390=AXIS2_PLACEMENT_3D('',#9463,#7816,#7817);
#6391=AXIS2_PLACEMENT_3D('',#9464,#7818,#7819);
#6392=AXIS2_PLACEMENT_3D('',#9466,#7820,#7821);
#6393=AXIS2_PLACEMENT_3D('',#9468,#7823,#7824);
#6394=AXIS2_PLACEMENT_3D('',#9470,#7825,#7826);
#6395=AXIS2_PLACEMENT_3D('',#9473,#7828,#7829);
#6396=AXIS2_PLACEMENT_3D('',#9474,#7830,#7831);
#6397=AXIS2_PLACEMENT_3D('',#9477,#7833,#7834);
#6398=AXIS2_PLACEMENT_3D('',#9478,#7835,#7836);
#6399=AXIS2_PLACEMENT_3D('',#9479,#7837,#7838);
#6400=AXIS2_PLACEMENT_3D('',#9480,#7839,#7840);
#6401=AXIS2_PLACEMENT_3D('',#9481,#7841,#7842);
#6402=AXIS2_PLACEMENT_3D('',#9483,#7843,#7844);
#6403=AXIS2_PLACEMENT_3D('',#9486,#7846,#7847);
#6404=AXIS2_PLACEMENT_3D('',#9487,#7848,#7849);
#6405=AXIS2_PLACEMENT_3D('',#9489,#7850,#7851);
#6406=AXIS2_PLACEMENT_3D('',#9492,#7853,#7854);
#6407=AXIS2_PLACEMENT_3D('',#9493,#7855,#7856);
#6408=AXIS2_PLACEMENT_3D('',#9495,#7857,#7858);
#6409=AXIS2_PLACEMENT_3D('',#9498,#7860,#7861);
#6410=AXIS2_PLACEMENT_3D('',#9499,#7862,#7863);
#6411=AXIS2_PLACEMENT_3D('',#9501,#7864,#7865);
#6412=AXIS2_PLACEMENT_3D('',#9504,#7867,#7868);
#6413=AXIS2_PLACEMENT_3D('',#9505,#7869,#7870);
#6414=AXIS2_PLACEMENT_3D('',#9507,#7871,#7872);
#6415=AXIS2_PLACEMENT_3D('',#9509,#7873,#7874);
#6416=AXIS2_PLACEMENT_3D('',#9510,#7875,#7876);
#6417=AXIS2_PLACEMENT_3D('',#9513,#7878,#7879);
#6418=AXIS2_PLACEMENT_3D('',#9514,#7880,#7881);
#6419=AXIS2_PLACEMENT_3D('',#9516,#7882,#7883);
#6420=AXIS2_PLACEMENT_3D('',#9519,#7885,#7886);
#6421=AXIS2_PLACEMENT_3D('',#9520,#7887,#7888);
#6422=AXIS2_PLACEMENT_3D('',#9522,#7889,#7890);
#6423=AXIS2_PLACEMENT_3D('',#9524,#7892,#7893);
#6424=AXIS2_PLACEMENT_3D('',#9525,#7894,#7895);
#6425=AXIS2_PLACEMENT_3D('',#9526,#7896,#7897);
#6426=AXIS2_PLACEMENT_3D('',#9527,#7898,#7899);
#6427=AXIS2_PLACEMENT_3D('',#9529,#7900,#7901);
#6428=AXIS2_PLACEMENT_3D('',#9530,#7902,#7903);
#6429=AXIS2_PLACEMENT_3D('',#9532,#7904,#7905);
#6430=AXIS2_PLACEMENT_3D('',#9534,#7907,#7908);
#6431=AXIS2_PLACEMENT_3D('',#9536,#7909,#7910);
#6432=AXIS2_PLACEMENT_3D('',#9538,#7912,#7913);
#6433=AXIS2_PLACEMENT_3D('',#9540,#7914,#7915);
#6434=AXIS2_PLACEMENT_3D('',#9542,#7917,#7918);
#6435=AXIS2_PLACEMENT_3D('',#9544,#7919,#7920);
#6436=AXIS2_PLACEMENT_3D('',#9545,#7921,#7922);
#6437=AXIS2_PLACEMENT_3D('',#9547,#7923,#7924);
#6438=AXIS2_PLACEMENT_3D('',#9549,#7926,#7927);
#6439=AXIS2_PLACEMENT_3D('',#9551,#7928,#7929);
#6440=AXIS2_PLACEMENT_3D('',#9553,#7931,#7932);
#6441=AXIS2_PLACEMENT_3D('',#9555,#7933,#7934);
#6442=AXIS2_PLACEMENT_3D('',#9557,#7936,#7937);
#6443=AXIS2_PLACEMENT_3D('',#9558,#7938,#7939);
#6444=AXIS2_PLACEMENT_3D('',#9567,#7944,#7945);
#6445=AXIS2_PLACEMENT_3D('',#9573,#7949,#7950);
#6446=AXIS2_PLACEMENT_3D('',#9579,#7954,#7955);
#6447=AXIS2_PLACEMENT_3D('',#9585,#7959,#7960);
#6448=AXIS2_PLACEMENT_3D('',#9591,#7964,#7965);
#6449=AXIS2_PLACEMENT_3D('',#9594,#7968,#7969);
#6450=AXIS2_PLACEMENT_3D('',#9595,#7970,#7971);
#6451=AXIS2_PLACEMENT_3D('',#9596,#7972,#7973);
#6452=AXIS2_PLACEMENT_3D('',#9597,#7974,#7975);
#6453=AXIS2_PLACEMENT_3D('',#9599,#7976,#7977);
#6454=AXIS2_PLACEMENT_3D('',#9602,#7979,#7980);
#6455=AXIS2_PLACEMENT_3D('',#9603,#7981,#7982);
#6456=AXIS2_PLACEMENT_3D('',#9605,#7983,#7984);
#6457=AXIS2_PLACEMENT_3D('',#9608,#7986,#7987);
#6458=AXIS2_PLACEMENT_3D('',#9609,#7988,#7989);
#6459=AXIS2_PLACEMENT_3D('',#9610,#7990,#7991);
#6460=AXIS2_PLACEMENT_3D('',#9611,#7992,#7993);
#6461=AXIS2_PLACEMENT_3D('',#9612,#7994,#7995);
#6462=AXIS2_PLACEMENT_3D('',#9624,#7997,#7998);
#6463=AXIS2_PLACEMENT_3D('',#9640,#7999,#8000);
#6464=AXIS2_PLACEMENT_3D('',#9642,#8001,#8002);
#6465=AXIS2_PLACEMENT_3D('',#9668,#8004,#8005);
#6466=AXIS2_PLACEMENT_3D('',#9671,#8008,#8009);
#6467=AXIS2_PLACEMENT_3D('',#9673,#8011,#8012);
#6468=AXIS2_PLACEMENT_3D('',#9675,#8014,#8015);
#6469=AXIS2_PLACEMENT_3D('',#9677,#8016,#8017);
#6470=AXIS2_PLACEMENT_3D('',#9680,#8019,#8020);
#6471=AXIS2_PLACEMENT_3D('',#9681,#8021,#8022);
#6472=AXIS2_PLACEMENT_3D('',#9683,#8024,#8025);
#6473=AXIS2_PLACEMENT_3D('',#9685,#8027,#8028);
#6474=AXIS2_PLACEMENT_3D('',#9686,#8029,#8030);
#6475=AXIS2_PLACEMENT_3D('',#9687,#8031,#8032);
#6476=AXIS2_PLACEMENT_3D('',#9688,#8033,#8034);
#6477=AXIS2_PLACEMENT_3D('',#9689,#8035,#8036);
#6478=AXIS2_PLACEMENT_3D('',#9690,#8037,#8038);
#6479=AXIS2_PLACEMENT_3D('',#9691,#8039,#8040);
#6480=AXIS2_PLACEMENT_3D('',#9692,#8041,#8042);
#6481=AXIS2_PLACEMENT_3D('',#9693,#8043,#8044);
#6482=AXIS2_PLACEMENT_3D('',#9694,#8045,#8046);
#6483=AXIS2_PLACEMENT_3D('',#9695,#8047,#8048);
#6484=AXIS2_PLACEMENT_3D('',#9696,#8049,#8050);
#6485=AXIS2_PLACEMENT_3D('',#9697,#8051,#8052);
#6486=AXIS2_PLACEMENT_3D('',#9698,#8053,#8054);
#6487=AXIS2_PLACEMENT_3D('',#9699,#8055,#8056);
#6488=AXIS2_PLACEMENT_3D('',#9700,#8057,#8058);
#6489=AXIS2_PLACEMENT_3D('',#9701,#8059,#8060);
#6490=AXIS2_PLACEMENT_3D('',#9702,#8061,#8062);
#6491=AXIS2_PLACEMENT_3D('',#9703,#8063,#8064);
#6492=AXIS2_PLACEMENT_3D('',#9704,#8065,#8066);
#6493=AXIS2_PLACEMENT_3D('',#9705,#8067,#8068);
#6494=AXIS2_PLACEMENT_3D('',#9706,#8069,#8070);
#6495=AXIS2_PLACEMENT_3D('',#9707,#8071,#8072);
#6496=AXIS2_PLACEMENT_3D('',#9708,#8073,#8074);
#6497=AXIS2_PLACEMENT_3D('',#9709,#8075,#8076);
#6498=AXIS2_PLACEMENT_3D('',#9710,#8077,#8078);
#6499=AXIS2_PLACEMENT_3D('',#9711,#8079,#8080);
#6500=AXIS2_PLACEMENT_3D('',#9712,#8081,#8082);
#6501=AXIS2_PLACEMENT_3D('',#9713,#8083,#8084);
#6502=AXIS2_PLACEMENT_3D('',#9714,#8085,#8086);
#6503=AXIS2_PLACEMENT_3D('',#9715,#8087,#8088);
#6504=AXIS2_PLACEMENT_3D('',#9716,#8089,#8090);
#6505=AXIS2_PLACEMENT_3D('',#9717,#8091,#8092);
#6506=AXIS2_PLACEMENT_3D('',#9718,#8093,#8094);
#6507=AXIS2_PLACEMENT_3D('',#9719,#8095,#8096);
#6508=AXIS2_PLACEMENT_3D('',#9720,#8097,#8098);
#6509=AXIS2_PLACEMENT_3D('',#9721,#8099,#8100);
#6510=AXIS2_PLACEMENT_3D('',#9722,#8101,#8102);
#6511=AXIS2_PLACEMENT_3D('',#9725,#8103,#8104);
#6512=AXIS2_PLACEMENT_3D('',#9731,#8108,#8109);
#6513=AXIS2_PLACEMENT_3D('',#9733,#8110,#8111);
#6514=AXIS2_PLACEMENT_3D('',#9738,#8114,#8115);
#6515=AXIS2_PLACEMENT_3D('',#9739,#8116,#8117);
#6516=AXIS2_PLACEMENT_3D('',#9741,#8118,#8119);
#6517=AXIS2_PLACEMENT_3D('',#9745,#8122,#8123);
#6518=AXIS2_PLACEMENT_3D('',#9746,#8124,#8125);
#6519=AXIS2_PLACEMENT_3D('',#9748,#8127,#8128);
#6520=AXIS2_PLACEMENT_3D('',#9749,#8129,#8130);
#6521=AXIS2_PLACEMENT_3D('',#9751,#8131,#8132);
#6522=AXIS2_PLACEMENT_3D('',#9754,#8134,#8135);
#6523=AXIS2_PLACEMENT_3D('',#9755,#8136,#8137);
#6524=AXIS2_PLACEMENT_3D('',#9757,#8138,#8139);
#6525=AXIS2_PLACEMENT_3D('',#9758,#8140,#8141);
#6526=AXIS2_PLACEMENT_3D('',#9759,#8142,#8143);
#6527=AXIS2_PLACEMENT_3D('',#9761,#8144,#8145);
#6528=AXIS2_PLACEMENT_3D('',#9764,#8147,#8148);
#6529=AXIS2_PLACEMENT_3D('',#9765,#8149,#8150);
#6530=AXIS2_PLACEMENT_3D('',#9766,#8151,#8152);
#6531=AXIS2_PLACEMENT_3D('',#9769,#8153,#8154);
#6532=AXIS2_PLACEMENT_3D('',#9773,#8157,#8158);
#6533=AXIS2_PLACEMENT_3D('',#9776,#8159,#8160);
#6534=AXIS2_PLACEMENT_3D('',#9780,#8163,#8164);
#6535=AXIS2_PLACEMENT_3D('',#9783,#8165,#8166);
#6536=AXIS2_PLACEMENT_3D('',#9787,#8169,#8170);
#6537=AXIS2_PLACEMENT_3D('',#9790,#8171,#8172);
#6538=AXIS2_PLACEMENT_3D('',#9794,#8175,#8176);
#6539=AXIS2_PLACEMENT_3D('',#9801,#8181,#8182);
#6540=AXIS2_PLACEMENT_3D('',#9806,#8186,#8187);
#6541=AXIS2_PLACEMENT_3D('',#9811,#8191,#8192);
#6542=AXIS2_PLACEMENT_3D('',#9814,#8195,#8196);
#6543=AXIS2_PLACEMENT_3D('',#9815,#8197,#8198);
#6544=AXIS2_PLACEMENT_3D('',#9816,#8199,#8200);
#6545=AXIS2_PLACEMENT_3D('',#9817,#8201,#8202);
#6546=AXIS2_PLACEMENT_3D('',#9819,#8203,#8204);
#6547=AXIS2_PLACEMENT_3D('',#9820,#8205,#8206);
#6548=AXIS2_PLACEMENT_3D('',#9821,#8207,#8208);
#6549=AXIS2_PLACEMENT_3D('',#9822,#8209,#8210);
#6550=AXIS2_PLACEMENT_3D('',#9823,#8211,#8212);
#6551=AXIS2_PLACEMENT_3D('',#9824,#8213,#8214);
#6552=AXIS2_PLACEMENT_3D('',#9825,#8215,#8216);
#6553=AXIS2_PLACEMENT_3D('',#9834,#8221,#8222);
#6554=AXIS2_PLACEMENT_3D('',#9840,#8226,#8227);
#6555=AXIS2_PLACEMENT_3D('',#9846,#8231,#8232);
#6556=AXIS2_PLACEMENT_3D('',#9849,#8235,#8236);
#6557=AXIS2_PLACEMENT_3D('',#9850,#8237,#8238);
#6558=AXIS2_PLACEMENT_3D('',#9853,#8240,#8241);
#6559=AXIS2_PLACEMENT_3D('',#9854,#8242,#8243);
#6560=AXIS2_PLACEMENT_3D('',#9855,#8244,#8245);
#6561=AXIS2_PLACEMENT_3D('',#9856,#8246,#8247);
#6562=AXIS2_PLACEMENT_3D('',#9865,#8252,#8253);
#6563=AXIS2_PLACEMENT_3D('',#9871,#8257,#8258);
#6564=AXIS2_PLACEMENT_3D('',#9877,#8262,#8263);
#6565=AXIS2_PLACEMENT_3D('',#9880,#8266,#8267);
#6566=AXIS2_PLACEMENT_3D('',#9889,#8272,#8273);
#6567=AXIS2_PLACEMENT_3D('',#9895,#8277,#8278);
#6568=AXIS2_PLACEMENT_3D('',#9901,#8282,#8283);
#6569=AXIS2_PLACEMENT_3D('',#9904,#8286,#8287);
#6570=AXIS2_PLACEMENT_3D('',#9905,#8288,#8289);
#6571=AXIS2_PLACEMENT_3D('',#9906,#8290,#8291);
#6572=AXIS2_PLACEMENT_3D('',#9907,#8292,#8293);
#6573=AXIS2_PLACEMENT_3D('',#9909,#8294,#8295);
#6574=AXIS2_PLACEMENT_3D('',#9912,#8297,#8298);
#6575=AXIS2_PLACEMENT_3D('',#9913,#8299,#8300);
#6576=AXIS2_PLACEMENT_3D('',#9915,#8301,#8302);
#6577=AXIS2_PLACEMENT_3D('',#9918,#8304,#8305);
#6578=AXIS2_PLACEMENT_3D('',#9919,#8306,#8307);
#6579=AXIS2_PLACEMENT_3D('',#9920,#8308,#8309);
#6580=AXIS2_PLACEMENT_3D('',#9921,#8310,#8311);
#6581=AXIS2_PLACEMENT_3D('',#9922,#8312,#8313);
#6582=AXIS2_PLACEMENT_3D('',#9931,#8318,#8319);
#6583=AXIS2_PLACEMENT_3D('',#9937,#8323,#8324);
#6584=AXIS2_PLACEMENT_3D('',#9943,#8328,#8329);
#6585=AXIS2_PLACEMENT_3D('',#9946,#8332,#8333);
#6586=AXIS2_PLACEMENT_3D('',#9947,#8334,#8335);
#6587=AXIS2_PLACEMENT_3D('',#9948,#8336,#8337);
#6588=AXIS2_PLACEMENT_3D('',#9949,#8338,#8339);
#6589=AXIS2_PLACEMENT_3D('',#9958,#8344,#8345);
#6590=AXIS2_PLACEMENT_3D('',#9964,#8349,#8350);
#6591=AXIS2_PLACEMENT_3D('',#9970,#8354,#8355);
#6592=AXIS2_PLACEMENT_3D('',#9976,#8359,#8360);
#6593=AXIS2_PLACEMENT_3D('',#9982,#8364,#8365);
#6594=AXIS2_PLACEMENT_3D('',#9985,#8368,#8369);
#6595=AXIS2_PLACEMENT_3D('',#9986,#8370,#8371);
#6596=AXIS2_PLACEMENT_3D('',#9987,#8372,#8373);
#6597=AXIS2_PLACEMENT_3D('',#9989,#8374,#8375);
#6598=AXIS2_PLACEMENT_3D('',#9990,#8376,#8377);
#6599=AXIS2_PLACEMENT_3D('',#9992,#8378,#8379);
#6600=AXIS2_PLACEMENT_3D('',#9993,#8380,#8381);
#6601=AXIS2_PLACEMENT_3D('',#9995,#8382,#8383);
#6602=AXIS2_PLACEMENT_3D('',#9997,#8385,#8386);
#6603=AXIS2_PLACEMENT_3D('',#9999,#8387,#8388);
#6604=AXIS2_PLACEMENT_3D('',#10001,#8390,#8391);
#6605=AXIS2_PLACEMENT_3D('',#10003,#8392,#8393);
#6606=AXIS2_PLACEMENT_3D('',#10005,#8395,#8396);
#6607=AXIS2_PLACEMENT_3D('',#10007,#8397,#8398);
#6608=AXIS2_PLACEMENT_3D('',#10008,#8399,#8400);
#6609=AXIS2_PLACEMENT_3D('',#10010,#8401,#8402);
#6610=AXIS2_PLACEMENT_3D('',#10012,#8404,#8405);
#6611=AXIS2_PLACEMENT_3D('',#10014,#8407,#8408);
#6612=AXIS2_PLACEMENT_3D('',#10015,#8409,#8410);
#6613=AXIS2_PLACEMENT_3D('',#10016,#8411,#8412);
#6614=AXIS2_PLACEMENT_3D('',#10017,#8413,#8414);
#6615=AXIS2_PLACEMENT_3D('',#10018,#8415,#8416);
#6616=AXIS2_PLACEMENT_3D('',#10019,#8417,#8418);
#6617=AXIS2_PLACEMENT_3D('',#10020,#8419,#8420);
#6618=AXIS2_PLACEMENT_3D('',#10021,#8421,#8422);
#6619=DIRECTION('axis',(0.,0.,1.));
#6620=DIRECTION('refdir',(1.,0.,0.));
#6621=DIRECTION('axis',(0.,0.,1.));
#6622=DIRECTION('refdir',(1.,0.,0.));
#6623=DIRECTION('axis',(0.,0.,1.));
#6624=DIRECTION('refdir',(1.,0.,0.));
#6625=DIRECTION('axis',(0.,0.,1.));
#6626=DIRECTION('refdir',(1.,0.,0.));
#6627=DIRECTION('center_axis',(0.,0.,1.));
#6628=DIRECTION('ref_axis',(1.,0.,0.));
#6629=DIRECTION('center_axis',(0.,0.,1.));
#6630=DIRECTION('ref_axis',(1.,0.,0.));
#6631=DIRECTION('',(0.,0.,1.));
#6632=DIRECTION('center_axis',(0.,0.,-1.));
#6633=DIRECTION('ref_axis',(1.,0.,0.));
#6634=DIRECTION('center_axis',(0.,0.,1.));
#6635=DIRECTION('ref_axis',(1.,0.,0.));
#6636=DIRECTION('center_axis',(0.,0.,1.));
#6637=DIRECTION('ref_axis',(1.,0.,0.));
#6638=DIRECTION('center_axis',(0.,0.,1.));
#6639=DIRECTION('ref_axis',(1.,0.,0.));
#6640=DIRECTION('',(0.,0.,1.));
#6641=DIRECTION('center_axis',(0.,0.,-1.));
#6642=DIRECTION('ref_axis',(1.,0.,0.));
#6643=DIRECTION('center_axis',(0.,0.,1.));
#6644=DIRECTION('ref_axis',(1.,0.,0.));
#6645=DIRECTION('center_axis',(0.,1.,0.));
#6646=DIRECTION('ref_axis',(1.,0.,0.));
#6647=DIRECTION('center_axis',(0.,1.,0.));
#6648=DIRECTION('ref_axis',(1.,0.,0.));
#6649=DIRECTION('',(0.,1.,0.));
#6650=DIRECTION('center_axis',(0.,-1.,0.));
#6651=DIRECTION('ref_axis',(1.,0.,0.));
#6652=DIRECTION('center_axis',(0.,1.,0.));
#6653=DIRECTION('ref_axis',(1.,0.,0.));
#6654=DIRECTION('center_axis',(0.,1.,0.));
#6655=DIRECTION('ref_axis',(1.,0.,0.));
#6656=DIRECTION('',(0.,1.,0.));
#6657=DIRECTION('center_axis',(0.,-1.,0.));
#6658=DIRECTION('ref_axis',(1.,0.,0.));
#6659=DIRECTION('center_axis',(0.,1.,0.));
#6660=DIRECTION('ref_axis',(1.,0.,0.));
#6661=DIRECTION('center_axis',(0.,1.,0.));
#6662=DIRECTION('ref_axis',(1.,0.,0.));
#6663=DIRECTION('',(0.,1.,0.));
#6664=DIRECTION('center_axis',(0.,-1.,0.));
#6665=DIRECTION('ref_axis',(1.,0.,0.));
#6666=DIRECTION('center_axis',(0.,1.,0.));
#6667=DIRECTION('ref_axis',(1.,0.,0.));
#6668=DIRECTION('center_axis',(0.,1.,0.));
#6669=DIRECTION('ref_axis',(1.,0.,0.));
#6670=DIRECTION('',(0.,1.,0.));
#6671=DIRECTION('center_axis',(0.,-1.,0.));
#6672=DIRECTION('ref_axis',(1.,0.,0.));
#6673=DIRECTION('center_axis',(0.,0.,1.));
#6674=DIRECTION('ref_axis',(1.,0.,0.));
#6675=DIRECTION('',(0.,0.,1.));
#6676=DIRECTION('center_axis',(0.,0.,1.));
#6677=DIRECTION('ref_axis',(1.,0.,0.));
#6678=DIRECTION('',(0.,0.,-1.));
#6679=DIRECTION('center_axis',(0.,0.,-1.));
#6680=DIRECTION('ref_axis',(1.,0.,0.));
#6681=DIRECTION('center_axis',(0.,0.,1.));
#6682=DIRECTION('ref_axis',(1.,0.,0.));
#6683=DIRECTION('',(1.,0.,0.));
#6684=DIRECTION('center_axis',(0.,0.,1.));
#6685=DIRECTION('ref_axis',(0.,-1.,0.));
#6686=DIRECTION('',(1.,0.,0.));
#6687=DIRECTION('center_axis',(0.,0.,1.));
#6688=DIRECTION('ref_axis',(1.,0.,0.));
#6689=DIRECTION('',(-1.,0.,0.));
#6690=DIRECTION('',(0.,-1.,0.));
#6691=DIRECTION('',(1.,0.,0.));
#6692=DIRECTION('',(0.,1.,0.));
#6693=DIRECTION('',(-1.,0.,0.));
#6694=DIRECTION('center_axis',(0.,1.,0.));
#6695=DIRECTION('ref_axis',(1.,0.,0.));
#6696=DIRECTION('center_axis',(0.,1.,0.));
#6697=DIRECTION('ref_axis',(1.,0.,0.));
#6698=DIRECTION('',(0.,1.,0.));
#6699=DIRECTION('center_axis',(0.,-1.,0.));
#6700=DIRECTION('ref_axis',(1.,0.,0.));
#6701=DIRECTION('center_axis',(0.,1.,0.));
#6702=DIRECTION('ref_axis',(1.,0.,0.));
#6703=DIRECTION('center_axis',(0.,1.,0.));
#6704=DIRECTION('ref_axis',(1.,0.,0.));
#6705=DIRECTION('',(0.,1.,0.));
#6706=DIRECTION('center_axis',(0.,1.,0.));
#6707=DIRECTION('ref_axis',(1.,0.,0.));
#6708=DIRECTION('center_axis',(0.,1.,0.));
#6709=DIRECTION('ref_axis',(1.,0.,0.));
#6710=DIRECTION('center_axis',(0.,-1.,0.));
#6711=DIRECTION('ref_axis',(0.,0.,-1.));
#6712=DIRECTION('center_axis',(0.,1.,0.));
#6713=DIRECTION('ref_axis',(1.,0.,0.));
#6714=DIRECTION('center_axis',(6.12323399573677E-17,0.,1.));
#6715=DIRECTION('ref_axis',(1.,0.,0.));
#6716=DIRECTION('center_axis',(0.,-1.,0.));
#6717=DIRECTION('ref_axis',(0.,0.,-1.));
#6718=DIRECTION('center_axis',(0.,1.,0.));
#6719=DIRECTION('ref_axis',(-1.,0.,0.));
#6720=DIRECTION('',(0.,0.,1.));
#6721=DIRECTION('',(-1.,0.,0.));
#6722=DIRECTION('',(0.,0.,1.));
#6723=DIRECTION('center_axis',(1.,0.,0.));
#6724=DIRECTION('ref_axis',(0.,1.,0.));
#6725=DIRECTION('',(0.,1.,0.));
#6726=DIRECTION('',(0.,0.,1.));
#6727=DIRECTION('center_axis',(0.,-1.,0.));
#6728=DIRECTION('ref_axis',(1.,0.,0.));
#6729=DIRECTION('',(1.,0.,0.));
#6730=DIRECTION('',(0.,0.,1.));
#6731=DIRECTION('center_axis',(-1.,0.,0.));
#6732=DIRECTION('ref_axis',(0.,-1.,0.));
#6733=DIRECTION('',(0.,-1.,0.));
#6734=DIRECTION('center_axis',(0.,0.,1.));
#6735=DIRECTION('ref_axis',(1.,0.,0.));
#6736=DIRECTION('axis',(0.,0.,1.));
#6737=DIRECTION('refdir',(1.,0.,0.));
#6738=DIRECTION('center_axis',(0.,0.,1.));
#6739=DIRECTION('ref_axis',(1.,0.,0.));
#6740=DIRECTION('center_axis',(0.,0.,1.));
#6741=DIRECTION('ref_axis',(1.,0.,0.));
#6742=DIRECTION('',(0.,0.,1.));
#6743=DIRECTION('center_axis',(0.,0.,-1.));
#6744=DIRECTION('ref_axis',(1.,0.,0.));
#6745=DIRECTION('center_axis',(0.,0.,1.));
#6746=DIRECTION('ref_axis',(1.,0.,0.));
#6747=DIRECTION('center_axis',(0.,0.,1.));
#6748=DIRECTION('ref_axis',(1.,0.,0.));
#6749=DIRECTION('center_axis',(0.,0.,1.));
#6750=DIRECTION('ref_axis',(1.,0.,0.));
#6751=DIRECTION('',(0.,0.,1.));
#6752=DIRECTION('center_axis',(0.,0.,-1.));
#6753=DIRECTION('ref_axis',(1.,0.,0.));
#6754=DIRECTION('center_axis',(0.,0.,1.));
#6755=DIRECTION('ref_axis',(1.,0.,0.));
#6756=DIRECTION('center_axis',(0.,1.,0.));
#6757=DIRECTION('ref_axis',(1.,0.,0.));
#6758=DIRECTION('center_axis',(0.,1.,0.));
#6759=DIRECTION('ref_axis',(1.,0.,0.));
#6760=DIRECTION('',(0.,1.,0.));
#6761=DIRECTION('center_axis',(0.,-1.,0.));
#6762=DIRECTION('ref_axis',(1.,0.,0.));
#6763=DIRECTION('center_axis',(0.,1.,0.));
#6764=DIRECTION('ref_axis',(1.,0.,0.));
#6765=DIRECTION('center_axis',(0.,1.,0.));
#6766=DIRECTION('ref_axis',(1.,0.,0.));
#6767=DIRECTION('',(0.,1.,0.));
#6768=DIRECTION('center_axis',(0.,-1.,0.));
#6769=DIRECTION('ref_axis',(1.,0.,0.));
#6770=DIRECTION('center_axis',(0.,1.,0.));
#6771=DIRECTION('ref_axis',(1.,0.,0.));
#6772=DIRECTION('center_axis',(0.,1.,0.));
#6773=DIRECTION('ref_axis',(1.,0.,0.));
#6774=DIRECTION('',(0.,1.,0.));
#6775=DIRECTION('center_axis',(0.,-1.,0.));
#6776=DIRECTION('ref_axis',(1.,0.,0.));
#6777=DIRECTION('center_axis',(0.,1.,0.));
#6778=DIRECTION('ref_axis',(1.,0.,0.));
#6779=DIRECTION('center_axis',(0.,1.,0.));
#6780=DIRECTION('ref_axis',(1.,0.,0.));
#6781=DIRECTION('',(0.,1.,0.));
#6782=DIRECTION('center_axis',(0.,-1.,0.));
#6783=DIRECTION('ref_axis',(1.,0.,0.));
#6784=DIRECTION('center_axis',(0.,0.,1.));
#6785=DIRECTION('ref_axis',(1.,0.,0.));
#6786=DIRECTION('',(0.,0.,1.));
#6787=DIRECTION('center_axis',(0.,0.,1.));
#6788=DIRECTION('ref_axis',(1.,0.,0.));
#6789=DIRECTION('',(0.,0.,-1.));
#6790=DIRECTION('center_axis',(0.,0.,-1.));
#6791=DIRECTION('ref_axis',(1.,0.,0.));
#6792=DIRECTION('center_axis',(0.,0.,1.));
#6793=DIRECTION('ref_axis',(1.,0.,0.));
#6794=DIRECTION('',(-1.,0.,0.));
#6795=DIRECTION('center_axis',(0.,0.,1.));
#6796=DIRECTION('ref_axis',(0.,-1.,0.));
#6797=DIRECTION('',(-1.,0.,0.));
#6798=DIRECTION('center_axis',(0.,0.,1.));
#6799=DIRECTION('ref_axis',(1.,0.,0.));
#6800=DIRECTION('',(1.,0.,0.));
#6801=DIRECTION('',(0.,1.,0.));
#6802=DIRECTION('',(-1.,0.,0.));
#6803=DIRECTION('',(0.,-1.,0.));
#6804=DIRECTION('',(1.,0.,0.));
#6805=DIRECTION('center_axis',(0.,1.,0.));
#6806=DIRECTION('ref_axis',(1.,0.,0.));
#6807=DIRECTION('center_axis',(0.,1.,0.));
#6808=DIRECTION('ref_axis',(1.,0.,0.));
#6809=DIRECTION('',(0.,1.,0.));
#6810=DIRECTION('center_axis',(0.,-1.,0.));
#6811=DIRECTION('ref_axis',(1.,0.,0.));
#6812=DIRECTION('center_axis',(0.,1.,0.));
#6813=DIRECTION('ref_axis',(1.,0.,0.));
#6814=DIRECTION('center_axis',(0.,1.,0.));
#6815=DIRECTION('ref_axis',(1.,0.,0.));
#6816=DIRECTION('',(0.,1.,0.));
#6817=DIRECTION('center_axis',(0.,1.,0.));
#6818=DIRECTION('ref_axis',(1.,0.,0.));
#6819=DIRECTION('center_axis',(0.,1.,0.));
#6820=DIRECTION('ref_axis',(1.,0.,0.));
#6821=DIRECTION('center_axis',(0.,1.,0.));
#6822=DIRECTION('ref_axis',(1.,0.,0.));
#6823=DIRECTION('center_axis',(0.,1.,0.));
#6824=DIRECTION('ref_axis',(0.,0.,1.));
#6825=DIRECTION('center_axis',(6.12323399573677E-17,0.,1.));
#6826=DIRECTION('ref_axis',(1.,0.,0.));
#6827=DIRECTION('center_axis',(0.,1.,0.));
#6828=DIRECTION('ref_axis',(0.,0.,1.));
#6829=DIRECTION('center_axis',(0.,1.,0.));
#6830=DIRECTION('ref_axis',(-1.,0.,0.));
#6831=DIRECTION('',(-1.,0.,0.));
#6832=DIRECTION('',(0.,0.,1.));
#6833=DIRECTION('',(0.,0.,1.));
#6834=DIRECTION('center_axis',(1.,0.,0.));
#6835=DIRECTION('ref_axis',(0.,1.,0.));
#6836=DIRECTION('',(0.,1.,0.));
#6837=DIRECTION('',(0.,0.,1.));
#6838=DIRECTION('center_axis',(0.,-1.,0.));
#6839=DIRECTION('ref_axis',(1.,0.,0.));
#6840=DIRECTION('',(0.,0.,1.));
#6841=DIRECTION('',(1.,0.,0.));
#6842=DIRECTION('center_axis',(-1.,0.,0.));
#6843=DIRECTION('ref_axis',(0.,-1.,0.));
#6844=DIRECTION('',(0.,-1.,0.));
#6845=DIRECTION('center_axis',(0.,0.,1.));
#6846=DIRECTION('ref_axis',(1.,0.,0.));
#6847=DIRECTION('axis',(0.,0.,1.));
#6848=DIRECTION('refdir',(1.,0.,0.));
#6849=DIRECTION('center_axis',(0.,1.,0.));
#6850=DIRECTION('ref_axis',(1.,0.,0.));
#6851=DIRECTION('center_axis',(0.,1.,0.));
#6852=DIRECTION('ref_axis',(1.,0.,0.));
#6853=DIRECTION('',(0.,1.,0.));
#6854=DIRECTION('center_axis',(0.,-1.,0.));
#6855=DIRECTION('ref_axis',(1.,0.,0.));
#6856=DIRECTION('center_axis',(0.,1.,0.));
#6857=DIRECTION('ref_axis',(1.,0.,0.));
#6858=DIRECTION('center_axis',(0.,1.,0.));
#6859=DIRECTION('ref_axis',(1.,0.,0.));
#6860=DIRECTION('',(0.,1.,0.));
#6861=DIRECTION('center_axis',(0.,-1.,0.));
#6862=DIRECTION('ref_axis',(1.,0.,0.));
#6863=DIRECTION('center_axis',(0.,1.,0.));
#6864=DIRECTION('ref_axis',(1.,0.,0.));
#6865=DIRECTION('center_axis',(0.,1.,0.));
#6866=DIRECTION('ref_axis',(1.,0.,0.));
#6867=DIRECTION('',(0.,1.,0.));
#6868=DIRECTION('center_axis',(0.,-1.,0.));
#6869=DIRECTION('ref_axis',(1.,0.,0.));
#6870=DIRECTION('center_axis',(0.,1.,0.));
#6871=DIRECTION('ref_axis',(1.,0.,0.));
#6872=DIRECTION('center_axis',(0.,1.,0.));
#6873=DIRECTION('ref_axis',(1.,0.,0.));
#6874=DIRECTION('',(0.,1.,0.));
#6875=DIRECTION('center_axis',(0.,-1.,0.));
#6876=DIRECTION('ref_axis',(1.,0.,0.));
#6877=DIRECTION('center_axis',(-1.,0.,0.));
#6878=DIRECTION('ref_axis',(0.,0.,1.));
#6879=DIRECTION('',(0.,0.,1.));
#6880=DIRECTION('',(0.,1.,0.));
#6881=DIRECTION('',(0.,0.,-1.));
#6882=DIRECTION('',(0.,1.,0.));
#6883=DIRECTION('center_axis',(0.,0.,-1.));
#6884=DIRECTION('ref_axis',(-1.,0.,0.));
#6885=DIRECTION('',(-1.,0.,0.));
#6886=DIRECTION('',(0.,1.,0.));
#6887=DIRECTION('',(1.,0.,0.));
#6888=DIRECTION('',(0.,1.,0.));
#6889=DIRECTION('center_axis',(0.,0.,-1.));
#6890=DIRECTION('ref_axis',(-1.,0.,0.));
#6891=DIRECTION('',(-1.,0.,0.));
#6892=DIRECTION('',(0.,-1.,0.));
#6893=DIRECTION('',(1.,0.,0.));
#6894=DIRECTION('center_axis',(1.,0.,0.));
#6895=DIRECTION('ref_axis',(0.,0.,-1.));
#6896=DIRECTION('',(0.,0.,-1.));
#6897=DIRECTION('',(0.,-1.,0.));
#6898=DIRECTION('',(0.,0.,1.));
#6899=DIRECTION('center_axis',(0.,1.,0.));
#6900=DIRECTION('ref_axis',(0.,0.,1.));
#6901=DIRECTION('center_axis',(0.,-1.,0.));
#6902=DIRECTION('ref_axis',(1.,0.,0.));
#6903=DIRECTION('',(1.,0.,0.));
#6904=DIRECTION('',(0.,0.,-1.));
#6905=DIRECTION('',(-1.,0.,0.));
#6906=DIRECTION('',(0.,0.,1.));
#6907=DIRECTION('',(1.,0.,0.));
#6908=DIRECTION('center_axis',(0.,0.,1.));
#6909=DIRECTION('ref_axis',(1.,0.,0.));
#6910=DIRECTION('',(-1.,0.,0.));
#6911=DIRECTION('',(0.,1.,0.));
#6912=DIRECTION('center_axis',(0.,0.,1.));
#6913=DIRECTION('ref_axis',(1.,0.,0.));
#6914=DIRECTION('',(0.,1.,0.));
#6915=DIRECTION('',(-1.,0.,0.));
#6916=DIRECTION('center_axis',(0.,1.,0.));
#6917=DIRECTION('ref_axis',(-1.83697019872103E-16,0.,-1.));
#6918=DIRECTION('center_axis',(0.,1.,0.));
#6919=DIRECTION('ref_axis',(1.,0.,0.));
#6920=DIRECTION('center_axis',(-1.,0.,0.));
#6921=DIRECTION('ref_axis',(0.,0.,1.));
#6922=DIRECTION('',(0.,0.,-1.));
#6923=DIRECTION('',(0.,1.,0.));
#6924=DIRECTION('center_axis',(0.,0.,-1.));
#6925=DIRECTION('ref_axis',(-1.,0.,0.));
#6926=DIRECTION('',(1.,0.,0.));
#6927=DIRECTION('',(0.,1.,0.));
#6928=DIRECTION('center_axis',(1.,0.,0.));
#6929=DIRECTION('ref_axis',(0.,0.,-1.));
#6930=DIRECTION('',(0.,0.,1.));
#6931=DIRECTION('center_axis',(0.,1.,0.));
#6932=DIRECTION('ref_axis',(1.,0.,0.));
#6933=DIRECTION('axis',(0.,0.,1.));
#6934=DIRECTION('refdir',(1.,0.,0.));
#6935=DIRECTION('center_axis',(0.,0.,1.));
#6936=DIRECTION('ref_axis',(1.,0.,0.));
#6937=DIRECTION('center_axis',(0.,0.,1.));
#6938=DIRECTION('ref_axis',(1.,0.,0.));
#6939=DIRECTION('center_axis',(0.,0.,1.));
#6940=DIRECTION('ref_axis',(1.,0.,0.));
#6941=DIRECTION('center_axis',(0.,0.,1.));
#6942=DIRECTION('ref_axis',(1.,0.,0.));
#6943=DIRECTION('center_axis',(0.,0.,1.));
#6944=DIRECTION('ref_axis',(1.,0.,0.));
#6945=DIRECTION('',(0.,0.,-1.));
#6946=DIRECTION('center_axis',(0.,0.,1.));
#6947=DIRECTION('ref_axis',(1.,0.,0.));
#6948=DIRECTION('center_axis',(0.,0.,-1.));
#6949=DIRECTION('ref_axis',(1.,0.,0.));
#6950=DIRECTION('center_axis',(0.,0.,1.));
#6951=DIRECTION('ref_axis',(1.,0.,0.));
#6952=DIRECTION('',(0.,0.,-1.));
#6953=DIRECTION('center_axis',(0.,0.,-1.));
#6954=DIRECTION('ref_axis',(1.,0.,0.));
#6955=DIRECTION('center_axis',(0.,0.,1.));
#6956=DIRECTION('ref_axis',(1.,0.,0.));
#6957=DIRECTION('',(0.,0.,-1.));
#6958=DIRECTION('center_axis',(0.,0.,1.));
#6959=DIRECTION('ref_axis',(1.,0.,0.));
#6960=DIRECTION('center_axis',(0.,0.,1.));
#6961=DIRECTION('ref_axis',(1.,0.,0.));
#6962=DIRECTION('axis',(0.,0.,1.));
#6963=DIRECTION('refdir',(1.,0.,0.));
#6964=DIRECTION('center_axis',(0.,0.,1.));
#6965=DIRECTION('ref_axis',(1.,0.,0.));
#6966=DIRECTION('center_axis',(1.22464679914735E-16,-1.,0.));
#6967=DIRECTION('ref_axis',(-1.,-1.22464679914735E-16,0.));
#6968=DIRECTION('center_axis',(0.,0.,-1.));
#6969=DIRECTION('ref_axis',(1.,0.,0.));
#6970=DIRECTION('axis',(0.,0.,1.));
#6971=DIRECTION('refdir',(1.,0.,0.));
#6972=DIRECTION('center_axis',(0.,0.,1.));
#6973=DIRECTION('ref_axis',(1.,0.,0.));
#6974=DIRECTION('center_axis',(0.,0.,1.));
#6975=DIRECTION('ref_axis',(1.,0.,0.));
#6976=DIRECTION('',(0.,0.,1.));
#6977=DIRECTION('center_axis',(0.,0.,1.));
#6978=DIRECTION('ref_axis',(1.,0.,0.));
#6979=DIRECTION('center_axis',(0.,0.,1.));
#6980=DIRECTION('ref_axis',(1.,0.,0.));
#6981=DIRECTION('center_axis',(0.,0.,-1.));
#6982=DIRECTION('ref_axis',(1.,0.,0.));
#6983=DIRECTION('center_axis',(0.,0.,1.));
#6984=DIRECTION('ref_axis',(1.,0.,0.));
#6985=DIRECTION('center_axis',(0.,0.,-1.));
#6986=DIRECTION('ref_axis',(1.,0.,0.));
#6987=DIRECTION('',(0.,0.,-1.));
#6988=DIRECTION('center_axis',(0.,0.,1.));
#6989=DIRECTION('ref_axis',(1.,0.,0.));
#6990=DIRECTION('center_axis',(0.,0.,1.));
#6991=DIRECTION('ref_axis',(1.,0.,0.));
#6992=DIRECTION('',(0.,0.,-1.));
#6993=DIRECTION('center_axis',(0.,0.,1.));
#6994=DIRECTION('ref_axis',(1.,0.,0.));
#6995=DIRECTION('center_axis',(0.,0.,1.));
#6996=DIRECTION('ref_axis',(1.,0.,0.));
#6997=DIRECTION('center_axis',(0.,0.,1.));
#6998=DIRECTION('ref_axis',(1.,0.,0.));
#6999=DIRECTION('axis',(0.,0.,1.));
#7000=DIRECTION('refdir',(1.,0.,0.));
#7001=DIRECTION('center_axis',(0.,0.,1.));
#7002=DIRECTION('ref_axis',(1.,0.,0.));
#7003=DIRECTION('center_axis',(0.,0.,1.));
#7004=DIRECTION('ref_axis',(1.,0.,0.));
#7005=DIRECTION('',(0.,0.,1.));
#7006=DIRECTION('center_axis',(0.,0.,-1.));
#7007=DIRECTION('ref_axis',(1.,0.,0.));
#7008=DIRECTION('center_axis',(0.,0.,1.));
#7009=DIRECTION('ref_axis',(1.,0.,0.));
#7010=DIRECTION('center_axis',(0.,0.,1.));
#7011=DIRECTION('ref_axis',(1.,0.,0.));
#7012=DIRECTION('center_axis',(0.,0.,1.));
#7013=DIRECTION('ref_axis',(1.,0.,0.));
#7014=DIRECTION('',(0.,0.,1.));
#7015=DIRECTION('center_axis',(0.,0.,-1.));
#7016=DIRECTION('ref_axis',(1.,0.,0.));
#7017=DIRECTION('center_axis',(0.,0.,1.));
#7018=DIRECTION('ref_axis',(1.,0.,0.));
#7019=DIRECTION('center_axis',(0.,0.,1.));
#7020=DIRECTION('ref_axis',(1.,0.,0.));
#7021=DIRECTION('center_axis',(0.,0.,1.));
#7022=DIRECTION('ref_axis',(1.,0.,0.));
#7023=DIRECTION('',(0.,0.,1.));
#7024=DIRECTION('center_axis',(0.,0.,-1.));
#7025=DIRECTION('ref_axis',(1.,0.,0.));
#7026=DIRECTION('center_axis',(0.,0.,1.));
#7027=DIRECTION('ref_axis',(1.,0.,0.));
#7028=DIRECTION('center_axis',(0.,0.,1.));
#7029=DIRECTION('ref_axis',(1.,0.,0.));
#7030=DIRECTION('',(0.,0.,1.));
#7031=DIRECTION('center_axis',(0.,0.,-1.));
#7032=DIRECTION('ref_axis',(1.,0.,0.));
#7033=DIRECTION('center_axis',(0.,0.,1.));
#7034=DIRECTION('ref_axis',(1.,0.,0.));
#7035=DIRECTION('center_axis',(0.,0.,1.));
#7036=DIRECTION('ref_axis',(1.,0.,0.));
#7037=DIRECTION('',(0.,0.,1.));
#7038=DIRECTION('center_axis',(0.,0.,-1.));
#7039=DIRECTION('ref_axis',(1.,0.,0.));
#7040=DIRECTION('center_axis',(0.,0.,1.));
#7041=DIRECTION('ref_axis',(1.,0.,0.));
#7042=DIRECTION('center_axis',(0.,0.,1.));
#7043=DIRECTION('ref_axis',(1.,0.,0.));
#7044=DIRECTION('',(0.,0.,1.));
#7045=DIRECTION('center_axis',(0.,0.,-1.));
#7046=DIRECTION('ref_axis',(1.,0.,0.));
#7047=DIRECTION('center_axis',(0.,0.,1.));
#7048=DIRECTION('ref_axis',(1.,0.,0.));
#7049=DIRECTION('center_axis',(0.,0.,1.));
#7050=DIRECTION('ref_axis',(1.,0.,0.));
#7051=DIRECTION('',(0.,0.,1.));
#7052=DIRECTION('center_axis',(0.,0.,-1.));
#7053=DIRECTION('ref_axis',(1.,0.,0.));
#7054=DIRECTION('center_axis',(0.,1.,0.));
#7055=DIRECTION('ref_axis',(-1.,0.,0.));
#7056=DIRECTION('',(-1.,0.,0.));
#7057=DIRECTION('',(0.,0.,1.));
#7058=DIRECTION('',(-1.,0.,0.));
#7059=DIRECTION('',(0.,0.,1.));
#7060=DIRECTION('center_axis',(1.,0.,0.));
#7061=DIRECTION('ref_axis',(0.,1.,0.));
#7062=DIRECTION('',(0.,1.,0.));
#7063=DIRECTION('',(0.,1.,0.));
#7064=DIRECTION('',(0.,0.,1.));
#7065=DIRECTION('center_axis',(0.,-1.,0.));
#7066=DIRECTION('ref_axis',(1.,0.,0.));
#7067=DIRECTION('',(1.,0.,0.));
#7068=DIRECTION('',(1.,0.,0.));
#7069=DIRECTION('',(0.,0.,1.));
#7070=DIRECTION('center_axis',(-1.,0.,0.));
#7071=DIRECTION('ref_axis',(0.,-1.,0.));
#7072=DIRECTION('',(0.,-1.,0.));
#7073=DIRECTION('',(0.,-1.,0.));
#7074=DIRECTION('center_axis',(0.,0.,1.));
#7075=DIRECTION('ref_axis',(1.,0.,0.));
#7076=DIRECTION('center_axis',(0.,0.,1.));
#7077=DIRECTION('ref_axis',(1.,0.,0.));
#7078=DIRECTION('axis',(0.,0.,1.));
#7079=DIRECTION('refdir',(1.,0.,0.));
#7080=DIRECTION('center_axis',(6.12323399573677E-17,0.,1.));
#7081=DIRECTION('ref_axis',(1.,0.,0.));
#7082=DIRECTION('center_axis',(0.,-1.,0.));
#7083=DIRECTION('ref_axis',(0.,0.,-1.));
#7084=DIRECTION('center_axis',(0.,1.,0.));
#7085=DIRECTION('ref_axis',(1.,0.,0.));
#7086=DIRECTION('center_axis',(0.,1.,0.));
#7087=DIRECTION('ref_axis',(1.,0.,0.));
#7088=DIRECTION('',(0.,-1.,0.));
#7089=DIRECTION('center_axis',(0.,-1.,0.));
#7090=DIRECTION('ref_axis',(1.,0.,0.));
#7091=DIRECTION('center_axis',(0.,1.,0.));
#7092=DIRECTION('ref_axis',(1.,0.,0.));
#7093=DIRECTION('center_axis',(0.,1.,0.));
#7094=DIRECTION('ref_axis',(1.,0.,0.));
#7095=DIRECTION('',(0.,-1.,0.));
#7096=DIRECTION('center_axis',(0.,1.,0.));
#7097=DIRECTION('ref_axis',(1.,0.,0.));
#7098=DIRECTION('center_axis',(0.,1.,0.));
#7099=DIRECTION('ref_axis',(1.,0.,0.));
#7100=DIRECTION('center_axis',(0.,1.,0.));
#7101=DIRECTION('ref_axis',(1.,0.,0.));
#7102=DIRECTION('axis',(0.,0.,1.));
#7103=DIRECTION('refdir',(1.,0.,0.));
#7104=DIRECTION('center_axis',(0.866025403784439,0.,-0.5));
#7105=DIRECTION('ref_axis',(0.5,0.,0.866025403784439));
#7106=DIRECTION('',(-0.5,0.,-0.866025403784439));
#7107=DIRECTION('',(0.,-1.,0.));
#7108=DIRECTION('',(0.5,0.,0.866025403784439));
#7109=DIRECTION('',(0.,-1.,0.));
#7110=DIRECTION('center_axis',(1.20185167898973E-16,0.,-1.));
#7111=DIRECTION('ref_axis',(1.,0.,1.20185167898973E-16));
#7112=DIRECTION('',(-1.,0.,-1.20185167898973E-16));
#7113=DIRECTION('',(0.,-1.,0.));
#7114=DIRECTION('',(1.,0.,1.20185167898973E-16));
#7115=DIRECTION('center_axis',(-0.866025403784439,0.,-0.5));
#7116=DIRECTION('ref_axis',(0.5,0.,-0.866025403784439));
#7117=DIRECTION('',(-0.5,0.,0.866025403784439));
#7118=DIRECTION('',(0.,-1.,0.));
#7119=DIRECTION('',(0.5,0.,-0.866025403784439));
#7120=DIRECTION('center_axis',(-0.866025403784439,0.,0.5));
#7121=DIRECTION('ref_axis',(-0.5,0.,-0.866025403784439));
#7122=DIRECTION('',(0.5,0.,0.866025403784439));
#7123=DIRECTION('',(0.,-1.,0.));
#7124=DIRECTION('',(-0.5,0.,-0.866025403784439));
#7125=DIRECTION('center_axis',(-2.40370335797945E-16,0.,1.));
#7126=DIRECTION('ref_axis',(-1.,0.,-2.40370335797945E-16));
#7127=DIRECTION('',(1.,0.,2.40370335797945E-16));
#7128=DIRECTION('',(0.,-1.,0.));
#7129=DIRECTION('',(-1.,0.,-2.40370335797945E-16));
#7130=DIRECTION('center_axis',(0.866025403784439,0.,0.5));
#7131=DIRECTION('ref_axis',(-0.5,0.,0.866025403784439));
#7132=DIRECTION('',(0.5,0.,-0.866025403784439));
#7133=DIRECTION('',(-0.5,0.,0.866025403784439));
#7134=DIRECTION('center_axis',(0.,1.,0.));
#7135=DIRECTION('ref_axis',(1.,0.,0.));
#7136=DIRECTION('center_axis',(0.,-1.,0.));
#7137=DIRECTION('ref_axis',(0.,0.,-1.));
#7138=DIRECTION('center_axis',(0.,1.,0.));
#7139=DIRECTION('ref_axis',(1.,0.,0.));
#7140=DIRECTION('center_axis',(0.,1.,0.));
#7141=DIRECTION('ref_axis',(1.,0.,0.));
#7142=DIRECTION('center_axis',(0.,1.,0.));
#7143=DIRECTION('ref_axis',(1.,0.,0.));
#7144=DIRECTION('center_axis',(0.,1.,0.));
#7145=DIRECTION('ref_axis',(1.,0.,0.));
#7146=DIRECTION('',(0.,-1.,0.));
#7147=DIRECTION('center_axis',(0.,1.,0.));
#7148=DIRECTION('ref_axis',(1.,0.,0.));
#7149=DIRECTION('center_axis',(0.,1.,0.));
#7150=DIRECTION('ref_axis',(1.,0.,0.));
#7151=DIRECTION('center_axis',(0.,1.,0.));
#7152=DIRECTION('ref_axis',(0.,0.,1.));
#7153=DIRECTION('center_axis',(0.,-1.,0.));
#7154=DIRECTION('ref_axis',(1.,0.,0.));
#7155=DIRECTION('center_axis',(0.,-1.,0.));
#7156=DIRECTION('ref_axis',(1.,0.,0.));
#7157=DIRECTION('center_axis',(0.,-1.,0.));
#7158=DIRECTION('ref_axis',(1.,0.,0.));
#7159=DIRECTION('',(0.707106781186548,0.707106781186547,8.65956056235493E-17));
#7160=DIRECTION('center_axis',(0.,-1.,0.));
#7161=DIRECTION('ref_axis',(1.,0.,0.));
#7162=DIRECTION('center_axis',(0.,-1.,0.));
#7163=DIRECTION('ref_axis',(1.,0.,0.));
#7164=DIRECTION('',(0.,1.,0.));
#7165=DIRECTION('center_axis',(0.,1.,0.));
#7166=DIRECTION('ref_axis',(1.,0.,0.));
#7167=DIRECTION('center_axis',(0.,-1.,0.));
#7168=DIRECTION('ref_axis',(1.,0.,0.));
#7169=DIRECTION('',(-0.707106781186547,0.707106781186548,-8.65956056235493E-17));
#7170=DIRECTION('center_axis',(0.,-1.,0.));
#7171=DIRECTION('ref_axis',(0.,0.,-1.));
#7172=DIRECTION('center_axis',(0.,-1.,0.));
#7173=DIRECTION('ref_axis',(1.,0.,0.));
#7174=DIRECTION('center_axis',(0.,1.,0.));
#7175=DIRECTION('ref_axis',(1.,0.,0.));
#7176=DIRECTION('center_axis',(0.,1.,0.));
#7177=DIRECTION('ref_axis',(1.,0.,0.));
#7178=DIRECTION('',(-0.447213595499958,0.894427190999916,-5.47678698264203E-17));
#7179=DIRECTION('center_axis',(0.,-1.,0.));
#7180=DIRECTION('ref_axis',(1.,0.,0.));
#7181=DIRECTION('',(0.,1.,0.));
#7182=DIRECTION('axis',(0.,0.,1.));
#7183=DIRECTION('refdir',(1.,0.,0.));
#7184=DIRECTION('center_axis',(0.,1.,0.));
#7185=DIRECTION('ref_axis',(1.,0.,0.));
#7186=DIRECTION('center_axis',(0.,1.,0.));
#7187=DIRECTION('ref_axis',(1.,0.,0.));
#7188=DIRECTION('',(0.707106781186548,-0.707106781186547,-8.65956056235494E-17));
#7189=DIRECTION('center_axis',(0.,-1.,0.));
#7190=DIRECTION('ref_axis',(1.,0.,0.));
#7191=DIRECTION('center_axis',(0.,1.,0.));
#7192=DIRECTION('ref_axis',(1.,0.,0.));
#7193=DIRECTION('',(0.,-1.,0.));
#7194=DIRECTION('center_axis',(0.,-1.,0.));
#7195=DIRECTION('ref_axis',(1.,0.,0.));
#7196=DIRECTION('center_axis',(0.,1.,0.));
#7197=DIRECTION('ref_axis',(1.,0.,0.));
#7198=DIRECTION('center_axis',(0.,1.,0.));
#7199=DIRECTION('ref_axis',(1.,0.,0.));
#7200=DIRECTION('center_axis',(0.,1.,0.));
#7201=DIRECTION('ref_axis',(1.,0.,0.));
#7202=DIRECTION('',(0.,-1.,0.));
#7203=DIRECTION('center_axis',(0.,1.,0.));
#7204=DIRECTION('ref_axis',(1.,0.,0.));
#7205=DIRECTION('center_axis',(0.,1.,0.));
#7206=DIRECTION('ref_axis',(1.,0.,0.));
#7207=DIRECTION('axis',(0.,0.,1.));
#7208=DIRECTION('refdir',(1.,0.,0.));
#7209=DIRECTION('center_axis',(0.,1.,0.));
#7210=DIRECTION('ref_axis',(1.,0.,0.));
#7211=DIRECTION('',(0.866025403784439,-0.5,1.06057523872491E-16));
#7212=DIRECTION('center_axis',(0.,-1.,0.));
#7213=DIRECTION('ref_axis',(1.,0.,0.));
#7214=DIRECTION('center_axis',(0.,-1.,0.));
#7215=DIRECTION('ref_axis',(1.,0.,0.));
#7216=DIRECTION('center_axis',(0.,1.,0.));
#7217=DIRECTION('ref_axis',(1.,0.,0.));
#7218=DIRECTION('',(-0.866025403784439,-0.5,-1.06057523872491E-16));
#7219=DIRECTION('center_axis',(1.20185167898973E-16,0.,-1.));
#7220=DIRECTION('ref_axis',(-1.,0.,-1.20185167898973E-16));
#7221=DIRECTION('',(0.,1.,0.));
#7222=DIRECTION('',(0.,1.,0.));
#7223=DIRECTION('center_axis',(-0.866025403784439,0.,-0.5));
#7224=DIRECTION('ref_axis',(-0.5,0.,0.866025403784439));
#7225=DIRECTION('',(0.,1.,0.));
#7226=DIRECTION('center_axis',(-0.866025403784439,0.,0.5));
#7227=DIRECTION('ref_axis',(0.5,0.,0.866025403784439));
#7228=DIRECTION('',(0.,1.,0.));
#7229=DIRECTION('center_axis',(0.,1.,0.));
#7230=DIRECTION('ref_axis',(1.,0.,0.));
#7231=DIRECTION('center_axis',(0.,1.,0.));
#7232=DIRECTION('ref_axis',(1.,0.,0.));
#7233=DIRECTION('',(0.,-1.,0.));
#7234=DIRECTION('center_axis',(0.,1.,0.));
#7235=DIRECTION('ref_axis',(1.,0.,0.));
#7236=DIRECTION('center_axis',(-2.40370335797945E-16,0.,1.));
#7237=DIRECTION('ref_axis',(1.,0.,2.40370335797945E-16));
#7238=DIRECTION('',(0.,1.,0.));
#7239=DIRECTION('center_axis',(0.866025403784439,0.,-0.5));
#7240=DIRECTION('ref_axis',(-0.5,0.,-0.866025403784439));
#7241=DIRECTION('',(0.,1.,0.));
#7242=DIRECTION('center_axis',(0.866025403784439,0.,0.5));
#7243=DIRECTION('ref_axis',(0.5,0.,-0.866025403784439));
#7244=DIRECTION('center_axis',(0.,1.,0.));
#7245=DIRECTION('ref_axis',(1.,0.,0.));
#7246=DIRECTION('center_axis',(0.,1.,0.));
#7247=DIRECTION('ref_axis',(1.,0.,0.));
#7248=DIRECTION('axis',(0.,0.,1.));
#7249=DIRECTION('refdir',(1.,0.,0.));
#7250=DIRECTION('center_axis',(0.,0.,1.));
#7251=DIRECTION('ref_axis',(1.,0.,0.));
#7252=DIRECTION('center_axis',(0.,0.,-1.));
#7253=DIRECTION('ref_axis',(1.,0.,0.));
#7254=DIRECTION('',(0.,0.,-1.));
#7255=DIRECTION('center_axis',(0.,0.,-1.));
#7256=DIRECTION('ref_axis',(1.,0.,0.));
#7257=DIRECTION('center_axis',(0.,0.,1.));
#7258=DIRECTION('ref_axis',(1.,0.,0.));
#7259=DIRECTION('center_axis',(0.,0.,1.));
#7260=DIRECTION('ref_axis',(1.,0.,0.));
#7261=DIRECTION('',(0.,0.,-1.));
#7262=DIRECTION('center_axis',(0.,0.,1.));
#7263=DIRECTION('ref_axis',(1.,0.,0.));
#7264=DIRECTION('center_axis',(0.,0.,1.));
#7265=DIRECTION('ref_axis',(1.,0.,0.));
#7266=DIRECTION('center_axis',(0.,0.,1.));
#7267=DIRECTION('ref_axis',(1.,0.,0.));
#7268=DIRECTION('axis',(0.,0.,1.));
#7269=DIRECTION('refdir',(1.,0.,0.));
#7270=DIRECTION('center_axis',(0.,1.,0.));
#7271=DIRECTION('ref_axis',(0.,0.,1.));
#7272=DIRECTION('center_axis',(0.,-1.,0.));
#7273=DIRECTION('ref_axis',(1.,0.,0.));
#7274=DIRECTION('center_axis',(0.,-1.,0.));
#7275=DIRECTION('ref_axis',(1.,0.,0.));
#7276=DIRECTION('center_axis',(0.,-1.,0.));
#7277=DIRECTION('ref_axis',(1.,0.,0.));
#7278=DIRECTION('',(0.707106781186547,0.707106781186548,8.65956056235493E-17));
#7279=DIRECTION('center_axis',(0.,-1.,0.));
#7280=DIRECTION('ref_axis',(1.,0.,0.));
#7281=DIRECTION('center_axis',(0.,-1.,0.));
#7282=DIRECTION('ref_axis',(1.,0.,0.));
#7283=DIRECTION('',(0.,1.,0.));
#7284=DIRECTION('center_axis',(0.,1.,0.));
#7285=DIRECTION('ref_axis',(1.,0.,0.));
#7286=DIRECTION('center_axis',(0.,-1.,0.));
#7287=DIRECTION('ref_axis',(1.,0.,0.));
#7288=DIRECTION('',(-0.707106781186547,0.707106781186548,-8.65956056235493E-17));
#7289=DIRECTION('center_axis',(0.,-1.,0.));
#7290=DIRECTION('ref_axis',(0.,0.,-1.));
#7291=DIRECTION('center_axis',(0.,-1.,0.));
#7292=DIRECTION('ref_axis',(1.,0.,0.));
#7293=DIRECTION('center_axis',(0.,1.,0.));
#7294=DIRECTION('ref_axis',(1.,0.,0.));
#7295=DIRECTION('center_axis',(0.,1.,0.));
#7296=DIRECTION('ref_axis',(1.,0.,0.));
#7297=DIRECTION('',(-0.447213595499958,0.894427190999916,-5.47678698264203E-17));
#7298=DIRECTION('center_axis',(0.,-1.,0.));
#7299=DIRECTION('ref_axis',(1.,0.,0.));
#7300=DIRECTION('center_axis',(0.,1.,0.));
#7301=DIRECTION('ref_axis',(1.,0.,0.));
#7302=DIRECTION('',(0.,1.,0.));
#7303=DIRECTION('center_axis',(0.,1.,0.));
#7304=DIRECTION('ref_axis',(1.,0.,0.));
#7305=DIRECTION('center_axis',(0.,-1.,0.));
#7306=DIRECTION('ref_axis',(1.,0.,0.));
#7307=DIRECTION('',(-0.707106781186547,0.707106781186548,-8.65956056235493E-17));
#7308=DIRECTION('center_axis',(0.,-1.,0.));
#7309=DIRECTION('ref_axis',(0.,0.,-1.));
#7310=DIRECTION('center_axis',(0.866025403784439,0.,-0.5));
#7311=DIRECTION('ref_axis',(0.5,0.,0.866025403784439));
#7312=DIRECTION('',(-0.5,0.,-0.866025403784439));
#7313=DIRECTION('',(0.,-1.,0.));
#7314=DIRECTION('',(0.5,0.,0.866025403784439));
#7315=DIRECTION('',(0.,-1.,0.));
#7316=DIRECTION('center_axis',(1.60246890531964E-16,0.,-1.));
#7317=DIRECTION('ref_axis',(1.,0.,1.60246890531964E-16));
#7318=DIRECTION('',(-1.,0.,-1.60246890531964E-16));
#7319=DIRECTION('',(0.,-1.,0.));
#7320=DIRECTION('',(1.,0.,1.60246890531964E-16));
#7321=DIRECTION('center_axis',(-0.866025403784439,0.,-0.5));
#7322=DIRECTION('ref_axis',(0.5,0.,-0.866025403784439));
#7323=DIRECTION('',(-0.5,0.,0.866025403784439));
#7324=DIRECTION('',(0.,-1.,0.));
#7325=DIRECTION('',(0.5,0.,-0.866025403784439));
#7326=DIRECTION('center_axis',(-0.866025403784439,0.,0.5));
#7327=DIRECTION('ref_axis',(-0.5,0.,-0.866025403784439));
#7328=DIRECTION('',(0.5,0.,0.866025403784439));
#7329=DIRECTION('',(0.,-1.,0.));
#7330=DIRECTION('',(-0.5,0.,-0.866025403784439));
#7331=DIRECTION('center_axis',(-1.60246890531964E-16,0.,1.));
#7332=DIRECTION('ref_axis',(-1.,0.,-1.60246890531964E-16));
#7333=DIRECTION('',(1.,0.,1.60246890531964E-16));
#7334=DIRECTION('',(0.,-1.,0.));
#7335=DIRECTION('',(-1.,0.,-1.60246890531964E-16));
#7336=DIRECTION('center_axis',(0.866025403784439,0.,0.5));
#7337=DIRECTION('ref_axis',(-0.5,0.,0.866025403784439));
#7338=DIRECTION('',(0.5,0.,-0.866025403784439));
#7339=DIRECTION('',(-0.5,0.,0.866025403784439));
#7340=DIRECTION('center_axis',(0.,1.,0.));
#7341=DIRECTION('ref_axis',(1.,0.,0.));
#7342=DIRECTION('center_axis',(0.,-1.,0.));
#7343=DIRECTION('ref_axis',(0.,0.,-1.));
#7344=DIRECTION('axis',(0.,0.,1.));
#7345=DIRECTION('refdir',(1.,0.,0.));
#7346=DIRECTION('center_axis',(0.,0.,1.));
#7347=DIRECTION('ref_axis',(1.,0.,0.));
#7348=DIRECTION('center_axis',(0.,0.,1.));
#7349=DIRECTION('ref_axis',(1.,0.,0.));
#7350=DIRECTION('',(0.,0.,-1.));
#7351=DIRECTION('center_axis',(0.,0.,1.));
#7352=DIRECTION('ref_axis',(1.,0.,0.));
#7353=DIRECTION('center_axis',(0.,0.,1.));
#7354=DIRECTION('ref_axis',(1.,0.,0.));
#7355=DIRECTION('center_axis',(0.,0.,1.));
#7356=DIRECTION('ref_axis',(1.,0.,0.));
#7357=DIRECTION('',(0.,0.,1.));
#7358=DIRECTION('',(1.,0.,0.));
#7359=DIRECTION('',(0.,0.,1.));
#7360=DIRECTION('',(1.,0.,0.));
#7361=DIRECTION('',(0.,0.,1.));
#7362=DIRECTION('',(1.,0.,0.));
#7363=DIRECTION('',(0.,0.,1.));
#7364=DIRECTION('',(1.,0.,0.));
#7365=DIRECTION('',(0.,0.,1.));
#7366=DIRECTION('',(1.,0.,0.));
#7367=DIRECTION('',(0.,0.,1.));
#7368=DIRECTION('',(1.,0.,0.));
#7369=DIRECTION('',(0.,0.,1.));
#7370=DIRECTION('',(1.,0.,0.));
#7371=DIRECTION('',(0.,0.,1.));
#7372=DIRECTION('',(1.,0.,0.));
#7373=DIRECTION('',(0.,0.,1.));
#7374=DIRECTION('',(-1.,1.22464679914735E-16,0.));
#7375=DIRECTION('',(0.,0.,1.));
#7376=DIRECTION('',(-1.,1.22464679914735E-16,0.));
#7377=DIRECTION('',(0.,0.,1.));
#7378=DIRECTION('',(-1.,1.22464679914735E-16,0.));
#7379=DIRECTION('',(0.,0.,1.));
#7380=DIRECTION('',(1.,0.,0.));
#7381=DIRECTION('',(0.,0.,1.));
#7382=DIRECTION('',(1.,0.,0.));
#7383=DIRECTION('',(0.,0.,1.));
#7384=DIRECTION('',(-1.,1.22464679914735E-16,0.));
#7385=DIRECTION('',(0.,0.,1.));
#7386=DIRECTION('',(-1.,1.22464679914735E-16,0.));
#7387=DIRECTION('',(0.,0.,1.));
#7388=DIRECTION('',(1.,0.,0.));
#7389=DIRECTION('',(0.,0.,1.));
#7390=DIRECTION('',(1.,0.,0.));
#7391=DIRECTION('',(0.,0.,1.));
#7392=DIRECTION('',(-1.,1.22464679914735E-16,0.));
#7393=DIRECTION('',(0.,0.,1.));
#7394=DIRECTION('',(-1.,1.22464679914735E-16,0.));
#7395=DIRECTION('',(0.,0.,1.));
#7396=DIRECTION('',(1.,0.,0.));
#7397=DIRECTION('',(0.,0.,1.));
#7398=DIRECTION('',(1.,0.,0.));
#7399=DIRECTION('',(0.,0.,1.));
#7400=DIRECTION('',(-1.,1.22464679914735E-16,0.));
#7401=DIRECTION('',(0.,0.,1.));
#7402=DIRECTION('',(-1.,1.22464679914735E-16,0.));
#7403=DIRECTION('',(0.,0.,1.));
#7404=DIRECTION('',(1.,0.,0.));
#7405=DIRECTION('',(0.,0.,1.));
#7406=DIRECTION('',(1.,0.,0.));
#7407=DIRECTION('',(0.,0.,1.));
#7408=DIRECTION('',(1.,0.,0.));
#7409=DIRECTION('',(0.,-1.,2.22044604925031E-16));
#7410=DIRECTION('',(1.,0.,0.));
#7411=DIRECTION('',(0.,0.,1.));
#7412=DIRECTION('',(1.,0.,0.));
#7413=DIRECTION('',(0.,-1.,2.22044604925031E-16));
#7414=DIRECTION('',(1.,0.,0.));
#7415=DIRECTION('',(0.,0.,1.));
#7416=DIRECTION('',(1.,0.,0.));
#7417=DIRECTION('',(0.,-1.,2.22044604925031E-16));
#7418=DIRECTION('',(1.,0.,0.));
#7419=DIRECTION('',(0.,0.,1.));
#7420=DIRECTION('',(1.,0.,0.));
#7421=DIRECTION('',(0.,-1.,2.22044604925031E-16));
#7422=DIRECTION('',(1.,0.,0.));
#7423=DIRECTION('',(0.,0.,1.));
#7424=DIRECTION('',(1.,0.,0.));
#7425=DIRECTION('',(0.,0.,1.));
#7426=DIRECTION('',(1.,0.,0.));
#7427=DIRECTION('axis',(0.,0.,1.));
#7428=DIRECTION('refdir',(1.,0.,0.));
#7429=DIRECTION('center_axis',(1.,0.,0.));
#7430=DIRECTION('ref_axis',(0.,0.,-1.));
#7431=DIRECTION('center_axis',(-1.,0.,0.));
#7432=DIRECTION('ref_axis',(0.,0.,-1.));
#7433=DIRECTION('',(-1.,0.,0.));
#7434=DIRECTION('center_axis',(-1.,0.,0.));
#7435=DIRECTION('ref_axis',(0.,0.,-1.));
#7436=DIRECTION('center_axis',(1.,0.,0.));
#7437=DIRECTION('ref_axis',(0.,0.,-1.));
#7438=DIRECTION('center_axis',(1.,0.,0.));
#7439=DIRECTION('ref_axis',(0.,0.,-1.));
#7440=DIRECTION('',(-1.,0.,0.));
#7441=DIRECTION('center_axis',(1.,0.,0.));
#7442=DIRECTION('ref_axis',(0.,0.,-1.));
#7443=DIRECTION('center_axis',(1.,0.,0.));
#7444=DIRECTION('ref_axis',(0.,0.,-1.));
#7445=DIRECTION('center_axis',(1.,0.,0.));
#7446=DIRECTION('ref_axis',(0.,0.,-1.));
#7447=DIRECTION('axis',(0.,0.,1.));
#7448=DIRECTION('refdir',(1.,0.,0.));
#7449=DIRECTION('center_axis',(0.,1.,0.));
#7450=DIRECTION('ref_axis',(1.,0.,0.));
#7451=DIRECTION('',(0.,0.,-1.));
#7452=DIRECTION('center_axis',(0.,1.,0.));
#7453=DIRECTION('ref_axis',(1.,0.,0.));
#7454=DIRECTION('',(0.,0.,1.));
#7455=DIRECTION('center_axis',(0.,-1.,0.));
#7456=DIRECTION('ref_axis',(1.,0.,0.));
#7457=DIRECTION('center_axis',(0.,1.,0.));
#7458=DIRECTION('ref_axis',(1.,0.,0.));
#7459=DIRECTION('center_axis',(0.,1.,0.));
#7460=DIRECTION('ref_axis',(1.,0.,0.));
#7461=DIRECTION('',(0.,1.,0.));
#7462=DIRECTION('center_axis',(0.707106781186548,-0.707106781186548,0.));
#7463=DIRECTION('ref_axis',(0.707106781186547,0.707106781186547,0.));
#7464=DIRECTION('center_axis',(-0.707106781186548,-0.707106781186548,0.));
#7465=DIRECTION('ref_axis',(0.707106781186547,-0.707106781186547,0.));
#7466=DIRECTION('center_axis',(0.,1.,0.));
#7467=DIRECTION('ref_axis',(1.,0.,0.));
#7468=DIRECTION('center_axis',(0.707106781186548,-0.707106781186548,0.));
#7469=DIRECTION('ref_axis',(0.707106781186547,0.707106781186547,0.));
#7470=DIRECTION('center_axis',(0.,1.,0.));
#7471=DIRECTION('ref_axis',(1.,0.,0.));
#7472=DIRECTION('',(0.,0.,-1.));
#7473=DIRECTION('center_axis',(0.,-1.,0.));
#7474=DIRECTION('ref_axis',(1.,0.,0.));
#7475=DIRECTION('',(0.,0.,1.));
#7476=DIRECTION('center_axis',(1.,0.,0.));
#7477=DIRECTION('ref_axis',(0.,0.,-1.));
#7478=DIRECTION('center_axis',(1.,0.,0.));
#7479=DIRECTION('ref_axis',(0.,0.,-1.));
#7480=DIRECTION('',(1.,0.,0.));
#7481=DIRECTION('center_axis',(-1.,0.,0.));
#7482=DIRECTION('ref_axis',(0.,0.,-1.));
#7483=DIRECTION('center_axis',(1.,0.,0.));
#7484=DIRECTION('ref_axis',(0.,0.,-1.));
#7485=DIRECTION('center_axis',(0.,1.,0.));
#7486=DIRECTION('ref_axis',(1.,0.,0.));
#7487=DIRECTION('center_axis',(0.707106781186548,-0.707106781186547,0.));
#7488=DIRECTION('ref_axis',(0.707106781186547,0.707106781186548,0.));
#7489=DIRECTION('center_axis',(-0.707106781186548,-0.707106781186547,0.));
#7490=DIRECTION('ref_axis',(0.707106781186547,-0.707106781186548,0.));
#7491=DIRECTION('center_axis',(1.,0.,0.));
#7492=DIRECTION('ref_axis',(0.,0.,-1.));
#7493=DIRECTION('center_axis',(1.,0.,0.));
#7494=DIRECTION('ref_axis',(0.,0.,-1.));
#7495=DIRECTION('center_axis',(0.,1.,0.));
#7496=DIRECTION('ref_axis',(1.,0.,0.));
#7497=DIRECTION('center_axis',(-0.707106781186548,-0.707106781186547,0.));
#7498=DIRECTION('ref_axis',(0.707106781186547,-0.707106781186548,0.));
#7499=DIRECTION('center_axis',(0.707106781186548,-0.707106781186547,0.));
#7500=DIRECTION('ref_axis',(0.707106781186547,0.707106781186548,0.));
#7501=DIRECTION('center_axis',(1.,0.,0.));
#7502=DIRECTION('ref_axis',(0.,0.,-1.));
#7503=DIRECTION('center_axis',(-1.,0.,0.));
#7504=DIRECTION('ref_axis',(0.,0.,-1.));
#7505=DIRECTION('center_axis',(1.,0.,0.));
#7506=DIRECTION('ref_axis',(0.,0.,-1.));
#7507=DIRECTION('center_axis',(1.,0.,0.));
#7508=DIRECTION('ref_axis',(0.,0.,-1.));
#7509=DIRECTION('center_axis',(1.,0.,0.));
#7510=DIRECTION('ref_axis',(0.,0.,-1.));
#7511=DIRECTION('center_axis',(1.,0.,0.));
#7512=DIRECTION('ref_axis',(0.,0.,-1.));
#7513=DIRECTION('',(1.,0.,0.));
#7514=DIRECTION('center_axis',(1.,0.,0.));
#7515=DIRECTION('ref_axis',(0.,1.,1.60812264967664E-16));
#7516=DIRECTION('center_axis',(-0.707106781186548,0.707106781186547,0.));
#7517=DIRECTION('ref_axis',(0.707106781186547,0.707106781186548,0.));
#7518=DIRECTION('',(-1.,0.,0.));
#7519=DIRECTION('center_axis',(0.707106781186548,0.707106781186547,0.));
#7520=DIRECTION('ref_axis',(0.707106781186547,-0.707106781186548,0.));
#7521=DIRECTION('center_axis',(0.707106781186548,0.707106781186547,0.));
#7522=DIRECTION('ref_axis',(0.707106781186547,-0.707106781186548,0.));
#7523=DIRECTION('',(1.,0.,0.));
#7524=DIRECTION('center_axis',(-0.707106781186548,0.707106781186547,0.));
#7525=DIRECTION('ref_axis',(0.707106781186547,0.707106781186548,0.));
#7526=DIRECTION('center_axis',(0.,1.,0.));
#7527=DIRECTION('ref_axis',(1.,0.,0.));
#7528=DIRECTION('center_axis',(0.,1.,0.));
#7529=DIRECTION('ref_axis',(1.,0.,0.));
#7530=DIRECTION('center_axis',(0.,1.,0.));
#7531=DIRECTION('ref_axis',(1.,0.,0.));
#7532=DIRECTION('center_axis',(0.,1.,0.));
#7533=DIRECTION('ref_axis',(1.,0.,0.));
#7534=DIRECTION('center_axis',(0.,1.,0.));
#7535=DIRECTION('ref_axis',(1.,0.,0.));
#7536=DIRECTION('center_axis',(0.,1.,0.));
#7537=DIRECTION('ref_axis',(1.,0.,0.));
#7538=DIRECTION('center_axis',(0.,1.,0.));
#7539=DIRECTION('ref_axis',(1.,0.,0.));
#7540=DIRECTION('center_axis',(0.707106781186548,0.707106781186547,0.));
#7541=DIRECTION('ref_axis',(0.707106781186547,-0.707106781186548,0.));
#7542=DIRECTION('center_axis',(-0.707106781186548,0.707106781186547,0.));
#7543=DIRECTION('ref_axis',(0.707106781186547,0.707106781186548,0.));
#7544=DIRECTION('',(0.,-1.,0.));
#7545=DIRECTION('center_axis',(0.,1.,0.));
#7546=DIRECTION('ref_axis',(1.,0.,0.));
#7547=DIRECTION('center_axis',(-0.707106781186548,0.707106781186547,0.));
#7548=DIRECTION('ref_axis',(0.707106781186547,0.707106781186548,0.));
#7549=DIRECTION('center_axis',(0.,1.,0.));
#7550=DIRECTION('ref_axis',(1.,0.,0.));
#7551=DIRECTION('center_axis',(1.,0.,0.));
#7552=DIRECTION('ref_axis',(0.,0.,-1.));
#7553=DIRECTION('center_axis',(1.,0.,0.));
#7554=DIRECTION('ref_axis',(0.,0.,-1.));
#7555=DIRECTION('',(-1.,0.,0.));
#7556=DIRECTION('',(-1.,0.,0.));
#7557=DIRECTION('center_axis',(1.,0.,0.));
#7558=DIRECTION('ref_axis',(0.,0.,-1.));
#7559=DIRECTION('center_axis',(1.,0.,0.));
#7560=DIRECTION('ref_axis',(0.,0.,-1.));
#7561=DIRECTION('center_axis',(1.,0.,0.));
#7562=DIRECTION('ref_axis',(0.,0.,-1.));
#7563=DIRECTION('axis',(0.,0.,1.));
#7564=DIRECTION('refdir',(1.,0.,0.));
#7565=DIRECTION('center_axis',(1.,0.,0.));
#7566=DIRECTION('ref_axis',(0.,0.,-1.));
#7567=DIRECTION('center_axis',(-1.,0.,0.));
#7568=DIRECTION('ref_axis',(0.,0.,-1.));
#7569=DIRECTION('',(-1.,0.,0.));
#7570=DIRECTION('center_axis',(-1.,0.,0.));
#7571=DIRECTION('ref_axis',(0.,0.,-1.));
#7572=DIRECTION('center_axis',(1.,0.,0.));
#7573=DIRECTION('ref_axis',(0.,0.,-1.));
#7574=DIRECTION('center_axis',(1.,0.,0.));
#7575=DIRECTION('ref_axis',(0.,0.,-1.));
#7576=DIRECTION('',(-1.,0.,0.));
#7577=DIRECTION('center_axis',(1.,0.,0.));
#7578=DIRECTION('ref_axis',(0.,0.,-1.));
#7579=DIRECTION('center_axis',(1.,0.,0.));
#7580=DIRECTION('ref_axis',(0.,0.,-1.));
#7581=DIRECTION('center_axis',(1.,0.,0.));
#7582=DIRECTION('ref_axis',(0.,0.,-1.));
#7583=DIRECTION('axis',(0.,0.,1.));
#7584=DIRECTION('refdir',(1.,0.,0.));
#7585=DIRECTION('center_axis',(0.,1.,0.));
#7586=DIRECTION('ref_axis',(1.,0.,0.));
#7587=DIRECTION('center_axis',(0.,-1.,0.));
#7588=DIRECTION('ref_axis',(1.,0.,0.));
#7589=DIRECTION('',(0.,-1.,0.));
#7590=DIRECTION('center_axis',(0.,-1.,0.));
#7591=DIRECTION('ref_axis',(1.,0.,0.));
#7592=DIRECTION('center_axis',(0.,1.,0.));
#7593=DIRECTION('ref_axis',(1.,0.,0.));
#7594=DIRECTION('center_axis',(0.,1.,0.));
#7595=DIRECTION('ref_axis',(1.,0.,0.));
#7596=DIRECTION('',(0.,-1.,0.));
#7597=DIRECTION('center_axis',(0.,1.,0.));
#7598=DIRECTION('ref_axis',(1.,0.,0.));
#7599=DIRECTION('center_axis',(0.,1.,0.));
#7600=DIRECTION('ref_axis',(1.,0.,0.));
#7601=DIRECTION('center_axis',(0.,1.,0.));
#7602=DIRECTION('ref_axis',(1.,0.,0.));
#7603=DIRECTION('axis',(0.,0.,1.));
#7604=DIRECTION('refdir',(1.,0.,0.));
#7605=DIRECTION('center_axis',(1.,0.,0.));
#7606=DIRECTION('ref_axis',(0.,0.,-1.));
#7607=DIRECTION('center_axis',(-1.,0.,0.));
#7608=DIRECTION('ref_axis',(0.,0.,-1.));
#7609=DIRECTION('',(-1.,0.,0.));
#7610=DIRECTION('center_axis',(-1.,0.,0.));
#7611=DIRECTION('ref_axis',(0.,0.,-1.));
#7612=DIRECTION('center_axis',(1.,0.,0.));
#7613=DIRECTION('ref_axis',(0.,0.,-1.));
#7614=DIRECTION('center_axis',(1.,0.,0.));
#7615=DIRECTION('ref_axis',(0.,0.,-1.));
#7616=DIRECTION('',(-1.,0.,0.));
#7617=DIRECTION('center_axis',(1.,0.,0.));
#7618=DIRECTION('ref_axis',(0.,0.,-1.));
#7619=DIRECTION('center_axis',(1.,0.,0.));
#7620=DIRECTION('ref_axis',(0.,0.,-1.));
#7621=DIRECTION('center_axis',(1.,0.,0.));
#7622=DIRECTION('ref_axis',(0.,0.,-1.));
#7623=DIRECTION('axis',(0.,0.,1.));
#7624=DIRECTION('refdir',(1.,0.,0.));
#7625=DIRECTION('center_axis',(0.,1.,0.));
#7626=DIRECTION('ref_axis',(1.,0.,0.));
#7627=DIRECTION('center_axis',(-0.707106781186548,0.707106781186548,0.));
#7628=DIRECTION('ref_axis',(0.707106781186547,0.707106781186547,0.));
#7629=DIRECTION('center_axis',(0.,1.,0.));
#7630=DIRECTION('ref_axis',(1.,0.,0.));
#7631=DIRECTION('',(0.,1.,0.));
#7632=DIRECTION('center_axis',(0.,-1.,0.));
#7633=DIRECTION('ref_axis',(1.,0.,0.));
#7634=DIRECTION('center_axis',(0.,1.,0.));
#7635=DIRECTION('ref_axis',(1.,0.,0.));
#7636=DIRECTION('center_axis',(6.12323399573677E-17,0.,1.));
#7637=DIRECTION('ref_axis',(1.,0.,0.));
#7638=DIRECTION('center_axis',(-1.22464679914735E-16,1.,0.));
#7639=DIRECTION('ref_axis',(-1.,-1.22464679914735E-16,0.));
#7640=DIRECTION('center_axis',(1.,0.,0.));
#7641=DIRECTION('ref_axis',(0.,0.,-1.));
#7642=DIRECTION('center_axis',(1.,0.,0.));
#7643=DIRECTION('ref_axis',(0.,0.,-1.));
#7644=DIRECTION('center_axis',(1.,0.,0.));
#7645=DIRECTION('ref_axis',(0.,0.,-1.));
#7646=DIRECTION('',(1.,0.,0.));
#7647=DIRECTION('center_axis',(-1.,0.,0.));
#7648=DIRECTION('ref_axis',(0.,0.,-1.));
#7649=DIRECTION('center_axis',(0.,-1.,0.));
#7650=DIRECTION('ref_axis',(0.,0.,-1.));
#7651=DIRECTION('center_axis',(0.,-1.,0.));
#7652=DIRECTION('ref_axis',(1.,0.,0.));
#7653=DIRECTION('center_axis',(0.,-1.,0.));
#7654=DIRECTION('ref_axis',(1.,0.,0.));
#7655=DIRECTION('center_axis',(0.,-1.,0.));
#7656=DIRECTION('ref_axis',(1.,0.,0.));
#7657=DIRECTION('',(0.,-1.,0.));
#7658=DIRECTION('center_axis',(1.,0.,0.));
#7659=DIRECTION('ref_axis',(0.,1.,0.));
#7660=DIRECTION('center_axis',(1.,0.,0.));
#7661=DIRECTION('ref_axis',(0.,0.,-1.));
#7662=DIRECTION('',(1.,0.,0.));
#7663=DIRECTION('center_axis',(-1.,0.,0.));
#7664=DIRECTION('ref_axis',(0.,1.,0.));
#7665=DIRECTION('center_axis',(-1.,0.,0.));
#7666=DIRECTION('ref_axis',(0.,0.,1.));
#7667=DIRECTION('center_axis',(6.12323399573677E-17,0.,1.));
#7668=DIRECTION('ref_axis',(1.,0.,0.));
#7669=DIRECTION('center_axis',(0.,-1.,0.));
#7670=DIRECTION('ref_axis',(1.,0.,0.));
#7671=DIRECTION('center_axis',(0.,-1.,0.));
#7672=DIRECTION('ref_axis',(1.,0.,0.));
#7673=DIRECTION('center_axis',(1.,0.,0.));
#7674=DIRECTION('ref_axis',(0.,0.,-1.));
#7675=DIRECTION('center_axis',(1.,0.,0.));
#7676=DIRECTION('ref_axis',(0.,0.,-1.));
#7677=DIRECTION('center_axis',(0.,-1.,0.));
#7678=DIRECTION('ref_axis',(1.,0.,0.));
#7679=DIRECTION('center_axis',(0.707106781186548,-0.707106781186548,0.));
#7680=DIRECTION('ref_axis',(0.707106781186547,0.707106781186547,0.));
#7681=DIRECTION('',(0.,1.,0.));
#7682=DIRECTION('center_axis',(0.,-1.,0.));
#7683=DIRECTION('ref_axis',(1.,0.,0.));
#7684=DIRECTION('center_axis',(0.,1.,0.));
#7685=DIRECTION('ref_axis',(0.,0.,1.));
#7686=DIRECTION('center_axis',(0.,-1.,0.));
#7687=DIRECTION('ref_axis',(1.,0.,0.));
#7688=DIRECTION('center_axis',(0.,-1.,0.));
#7689=DIRECTION('ref_axis',(1.,0.,0.));
#7690=DIRECTION('center_axis',(0.,-1.,0.));
#7691=DIRECTION('ref_axis',(1.,0.,0.));
#7692=DIRECTION('',(0.,1.,0.));
#7693=DIRECTION('center_axis',(0.,-1.,0.));
#7694=DIRECTION('ref_axis',(0.,0.,-1.));
#7695=DIRECTION('center_axis',(-1.,0.,0.));
#7696=DIRECTION('ref_axis',(0.,0.,1.));
#7697=DIRECTION('center_axis',(1.,0.,0.));
#7698=DIRECTION('ref_axis',(0.,0.,-1.));
#7699=DIRECTION('center_axis',(1.,0.,0.));
#7700=DIRECTION('ref_axis',(0.,0.,-1.));
#7701=DIRECTION('center_axis',(1.,0.,0.));
#7702=DIRECTION('ref_axis',(0.,1.,0.));
#7703=DIRECTION('center_axis',(1.,0.,0.));
#7704=DIRECTION('ref_axis',(0.,0.,-1.));
#7705=DIRECTION('',(-1.,0.,0.));
#7706=DIRECTION('center_axis',(1.,0.,0.));
#7707=DIRECTION('ref_axis',(0.,0.,-1.));
#7708=DIRECTION('center_axis',(1.,0.,0.));
#7709=DIRECTION('ref_axis',(0.,1.,0.));
#7710=DIRECTION('',(-1.,0.,0.));
#7711=DIRECTION('axis',(0.,0.,1.));
#7712=DIRECTION('refdir',(1.,0.,0.));
#7713=DIRECTION('center_axis',(0.,1.,0.));
#7714=DIRECTION('ref_axis',(1.,0.,0.));
#7715=DIRECTION('',(-0.5,0.,0.866025403784439));
#7716=DIRECTION('',(-1.,0.,-2.84883360945713E-16));
#7717=DIRECTION('',(-0.5,0.,-0.866025403784439));
#7718=DIRECTION('',(0.5,0.,-0.866025403784439));
#7719=DIRECTION('',(1.,0.,0.));
#7720=DIRECTION('',(0.5,0.,0.866025403784439));
#7721=DIRECTION('center_axis',(0.,-1.,0.));
#7722=DIRECTION('ref_axis',(1.,0.,0.));
#7723=DIRECTION('center_axis',(0.,1.,0.));
#7724=DIRECTION('ref_axis',(1.,0.,0.));
#7725=DIRECTION('',(0.5,0.,-0.866025403784439));
#7726=DIRECTION('',(-0.5,0.,-0.866025403784439));
#7727=DIRECTION('',(-1.,0.,0.));
#7728=DIRECTION('',(-0.5,0.,0.866025403784439));
#7729=DIRECTION('',(0.5,0.,0.866025403784439));
#7730=DIRECTION('',(1.,0.,2.84883360945713E-16));
#7731=DIRECTION('center_axis',(0.,1.,0.));
#7732=DIRECTION('ref_axis',(1.,0.,0.));
#7733=DIRECTION('center_axis',(-2.84883360945713E-16,0.,1.));
#7734=DIRECTION('ref_axis',(1.,0.,2.84883360945713E-16));
#7735=DIRECTION('',(0.,-1.,0.));
#7736=DIRECTION('',(0.,1.,0.));
#7737=DIRECTION('center_axis',(-0.866025403784439,0.,0.5));
#7738=DIRECTION('ref_axis',(0.5,0.,0.866025403784439));
#7739=DIRECTION('',(0.,1.,0.));
#7740=DIRECTION('center_axis',(-0.866025403784439,0.,-0.5));
#7741=DIRECTION('ref_axis',(-0.5,0.,0.866025403784439));
#7742=DIRECTION('',(0.,1.,0.));
#7743=DIRECTION('center_axis',(0.,0.,-1.));
#7744=DIRECTION('ref_axis',(-1.,0.,0.));
#7745=DIRECTION('',(0.,1.,0.));
#7746=DIRECTION('center_axis',(0.866025403784439,0.,-0.5));
#7747=DIRECTION('ref_axis',(-0.5,0.,-0.866025403784439));
#7748=DIRECTION('',(0.,1.,0.));
#7749=DIRECTION('center_axis',(0.866025403784439,0.,0.5));
#7750=DIRECTION('ref_axis',(0.5,0.,-0.866025403784439));
#7751=DIRECTION('center_axis',(0.,-1.,0.));
#7752=DIRECTION('ref_axis',(1.,0.,0.));
#7753=DIRECTION('',(0.,1.,0.));
#7754=DIRECTION('center_axis',(0.,-1.,0.));
#7755=DIRECTION('ref_axis',(1.,0.,0.));
#7756=DIRECTION('center_axis',(0.,1.,0.));
#7757=DIRECTION('ref_axis',(0.,0.,1.));
#7758=DIRECTION('center_axis',(0.,-1.,0.));
#7759=DIRECTION('ref_axis',(1.,0.,0.));
#7760=DIRECTION('center_axis',(0.,-1.,0.));
#7761=DIRECTION('ref_axis',(1.,0.,0.));
#7762=DIRECTION('center_axis',(0.,-1.,0.));
#7763=DIRECTION('ref_axis',(1.,0.,0.));
#7764=DIRECTION('',(0.707106781186547,0.707106781186548,8.65956056235493E-17));
#7765=DIRECTION('center_axis',(0.,-1.,0.));
#7766=DIRECTION('ref_axis',(1.,0.,0.));
#7767=DIRECTION('center_axis',(0.,-1.,0.));
#7768=DIRECTION('ref_axis',(1.,0.,0.));
#7769=DIRECTION('',(0.,1.,0.));
#7770=DIRECTION('center_axis',(0.,1.,0.));
#7771=DIRECTION('ref_axis',(1.,0.,0.));
#7772=DIRECTION('center_axis',(0.,-1.,0.));
#7773=DIRECTION('ref_axis',(1.,0.,0.));
#7774=DIRECTION('',(-0.707106781186547,0.707106781186548,-8.65956056235493E-17));
#7775=DIRECTION('center_axis',(0.,-1.,0.));
#7776=DIRECTION('ref_axis',(0.,0.,-1.));
#7777=DIRECTION('center_axis',(0.,-1.,0.));
#7778=DIRECTION('ref_axis',(1.,0.,0.));
#7779=DIRECTION('center_axis',(0.,-1.,0.));
#7780=DIRECTION('ref_axis',(1.,0.,0.));
#7781=DIRECTION('',(0.,1.,0.));
#7782=DIRECTION('axis',(0.,0.,1.));
#7783=DIRECTION('refdir',(1.,0.,0.));
#7784=DIRECTION('center_axis',(1.,0.,0.));
#7785=DIRECTION('ref_axis',(0.,0.,-1.));
#7786=DIRECTION('center_axis',(1.,0.,0.));
#7787=DIRECTION('ref_axis',(0.,0.,-1.));
#7788=DIRECTION('',(1.,0.,0.));
#7789=DIRECTION('center_axis',(-1.,0.,0.));
#7790=DIRECTION('ref_axis',(0.,0.,-1.));
#7791=DIRECTION('center_axis',(1.,0.,0.));
#7792=DIRECTION('ref_axis',(0.,0.,-1.));
#7793=DIRECTION('center_axis',(1.,0.,0.));
#7794=DIRECTION('ref_axis',(0.,0.,-1.));
#7795=DIRECTION('',(1.,0.,0.));
#7796=DIRECTION('center_axis',(-1.,0.,0.));
#7797=DIRECTION('ref_axis',(0.,0.,-1.));
#7798=DIRECTION('center_axis',(1.,0.,0.));
#7799=DIRECTION('ref_axis',(0.,0.,-1.));
#7800=DIRECTION('center_axis',(1.,0.,0.));
#7801=DIRECTION('ref_axis',(0.,0.,-1.));
#7802=DIRECTION('',(1.,0.,0.));
#7803=DIRECTION('center_axis',(-1.,0.,0.));
#7804=DIRECTION('ref_axis',(0.,0.,-1.));
#7805=DIRECTION('center_axis',(1.,0.,0.));
#7806=DIRECTION('ref_axis',(0.,0.,-1.));
#7807=DIRECTION('center_axis',(1.,0.,0.));
#7808=DIRECTION('ref_axis',(0.,0.,-1.));
#7809=DIRECTION('',(1.,0.,0.));
#7810=DIRECTION('center_axis',(-1.,0.,0.));
#7811=DIRECTION('ref_axis',(0.,0.,-1.));
#7812=DIRECTION('center_axis',(1.,0.,0.));
#7813=DIRECTION('ref_axis',(0.,0.,-1.));
#7814=DIRECTION('center_axis',(1.,0.,0.));
#7815=DIRECTION('ref_axis',(0.,0.,-1.));
#7816=DIRECTION('center_axis',(-1.,0.,0.));
#7817=DIRECTION('ref_axis',(0.,0.,-1.));
#7818=DIRECTION('center_axis',(1.,0.,0.));
#7819=DIRECTION('ref_axis',(0.,0.,-1.));
#7820=DIRECTION('center_axis',(1.,0.,0.));
#7821=DIRECTION('ref_axis',(0.,0.,-1.));
#7822=DIRECTION('',(-1.,0.,0.));
#7823=DIRECTION('center_axis',(1.,0.,0.));
#7824=DIRECTION('ref_axis',(0.,0.,-1.));
#7825=DIRECTION('center_axis',(-1.,0.,0.));
#7826=DIRECTION('ref_axis',(0.,0.,-1.));
#7827=DIRECTION('',(-1.,0.,0.));
#7828=DIRECTION('center_axis',(-1.,0.,0.));
#7829=DIRECTION('ref_axis',(0.,0.,-1.));
#7830=DIRECTION('center_axis',(1.,0.,0.));
#7831=DIRECTION('ref_axis',(0.,0.,-1.));
#7832=DIRECTION('',(-1.,0.,0.));
#7833=DIRECTION('center_axis',(1.,0.,0.));
#7834=DIRECTION('ref_axis',(0.,0.,-1.));
#7835=DIRECTION('center_axis',(1.,0.,0.));
#7836=DIRECTION('ref_axis',(0.,0.,-1.));
#7837=DIRECTION('center_axis',(1.,0.,0.));
#7838=DIRECTION('ref_axis',(0.,0.,-1.));
#7839=DIRECTION('axis',(0.,0.,1.));
#7840=DIRECTION('refdir',(1.,0.,0.));
#7841=DIRECTION('center_axis',(1.,0.,0.));
#7842=DIRECTION('ref_axis',(0.,0.,-1.));
#7843=DIRECTION('center_axis',(1.,0.,0.));
#7844=DIRECTION('ref_axis',(0.,0.,-1.));
#7845=DIRECTION('',(1.,0.,0.));
#7846=DIRECTION('center_axis',(-1.,0.,0.));
#7847=DIRECTION('ref_axis',(0.,0.,-1.));
#7848=DIRECTION('center_axis',(1.,0.,0.));
#7849=DIRECTION('ref_axis',(0.,0.,-1.));
#7850=DIRECTION('center_axis',(1.,0.,0.));
#7851=DIRECTION('ref_axis',(0.,0.,-1.));
#7852=DIRECTION('',(1.,0.,0.));
#7853=DIRECTION('center_axis',(-1.,0.,0.));
#7854=DIRECTION('ref_axis',(0.,0.,-1.));
#7855=DIRECTION('center_axis',(1.,0.,0.));
#7856=DIRECTION('ref_axis',(0.,0.,-1.));
#7857=DIRECTION('center_axis',(1.,0.,0.));
#7858=DIRECTION('ref_axis',(0.,0.,-1.));
#7859=DIRECTION('',(1.,0.,0.));
#7860=DIRECTION('center_axis',(-1.,0.,0.));
#7861=DIRECTION('ref_axis',(0.,0.,-1.));
#7862=DIRECTION('center_axis',(1.,0.,0.));
#7863=DIRECTION('ref_axis',(0.,0.,-1.));
#7864=DIRECTION('center_axis',(1.,0.,0.));
#7865=DIRECTION('ref_axis',(0.,0.,-1.));
#7866=DIRECTION('',(1.,0.,0.));
#7867=DIRECTION('center_axis',(-1.,0.,0.));
#7868=DIRECTION('ref_axis',(0.,0.,-1.));
#7869=DIRECTION('center_axis',(1.,0.,0.));
#7870=DIRECTION('ref_axis',(0.,0.,-1.));
#7871=DIRECTION('center_axis',(1.,0.,0.));
#7872=DIRECTION('ref_axis',(0.,0.,-1.));
#7873=DIRECTION('center_axis',(1.,0.,0.));
#7874=DIRECTION('ref_axis',(0.,0.,-1.));
#7875=DIRECTION('center_axis',(1.,0.,0.));
#7876=DIRECTION('ref_axis',(0.,0.,-1.));
#7877=DIRECTION('',(-1.,0.,0.));
#7878=DIRECTION('center_axis',(1.,0.,0.));
#7879=DIRECTION('ref_axis',(0.,0.,-1.));
#7880=DIRECTION('center_axis',(1.,0.,0.));
#7881=DIRECTION('ref_axis',(0.,0.,-1.));
#7882=DIRECTION('center_axis',(-1.,0.,0.));
#7883=DIRECTION('ref_axis',(0.,0.,-1.));
#7884=DIRECTION('',(-1.,0.,0.));
#7885=DIRECTION('center_axis',(-1.,0.,0.));
#7886=DIRECTION('ref_axis',(0.,0.,-1.));
#7887=DIRECTION('center_axis',(1.,0.,0.));
#7888=DIRECTION('ref_axis',(0.,0.,-1.));
#7889=DIRECTION('center_axis',(1.,0.,0.));
#7890=DIRECTION('ref_axis',(0.,0.,-1.));
#7891=DIRECTION('',(-1.,0.,0.));
#7892=DIRECTION('center_axis',(1.,0.,0.));
#7893=DIRECTION('ref_axis',(0.,0.,-1.));
#7894=DIRECTION('center_axis',(1.,0.,0.));
#7895=DIRECTION('ref_axis',(0.,0.,-1.));
#7896=DIRECTION('axis',(0.,0.,1.));
#7897=DIRECTION('refdir',(1.,0.,0.));
#7898=DIRECTION('center_axis',(0.,1.,0.));
#7899=DIRECTION('ref_axis',(0.,0.,1.));
#7900=DIRECTION('center_axis',(0.,-1.,0.));
#7901=DIRECTION('ref_axis',(1.,0.,0.));
#7902=DIRECTION('center_axis',(0.,-1.,0.));
#7903=DIRECTION('ref_axis',(1.,0.,0.));
#7904=DIRECTION('center_axis',(0.,-1.,0.));
#7905=DIRECTION('ref_axis',(1.,0.,0.));
#7906=DIRECTION('',(0.707106781186548,0.707106781186547,8.65956056235493E-17));
#7907=DIRECTION('center_axis',(0.,-1.,0.));
#7908=DIRECTION('ref_axis',(1.,0.,0.));
#7909=DIRECTION('center_axis',(0.,-1.,0.));
#7910=DIRECTION('ref_axis',(1.,0.,0.));
#7911=DIRECTION('',(0.,1.,0.));
#7912=DIRECTION('center_axis',(0.,1.,0.));
#7913=DIRECTION('ref_axis',(1.,0.,0.));
#7914=DIRECTION('center_axis',(0.,-1.,0.));
#7915=DIRECTION('ref_axis',(1.,0.,0.));
#7916=DIRECTION('',(-0.707106781186548,0.707106781186547,-8.65956056235494E-17));
#7917=DIRECTION('center_axis',(0.,-1.,0.));
#7918=DIRECTION('ref_axis',(0.,0.,-1.));
#7919=DIRECTION('center_axis',(0.,-1.,0.));
#7920=DIRECTION('ref_axis',(1.,0.,0.));
#7921=DIRECTION('center_axis',(0.,1.,0.));
#7922=DIRECTION('ref_axis',(1.,0.,0.));
#7923=DIRECTION('center_axis',(0.,1.,0.));
#7924=DIRECTION('ref_axis',(1.,0.,0.));
#7925=DIRECTION('',(-0.447213595499958,0.894427190999916,-5.47678698264203E-17));
#7926=DIRECTION('center_axis',(0.,-1.,0.));
#7927=DIRECTION('ref_axis',(1.,0.,0.));
#7928=DIRECTION('center_axis',(0.,1.,0.));
#7929=DIRECTION('ref_axis',(1.,0.,0.));
#7930=DIRECTION('',(0.,1.,0.));
#7931=DIRECTION('center_axis',(0.,1.,0.));
#7932=DIRECTION('ref_axis',(1.,0.,0.));
#7933=DIRECTION('center_axis',(0.,-1.,0.));
#7934=DIRECTION('ref_axis',(1.,0.,0.));
#7935=DIRECTION('',(-0.707106781186547,0.707106781186548,-8.65956056235493E-17));
#7936=DIRECTION('center_axis',(0.,-1.,0.));
#7937=DIRECTION('ref_axis',(0.,0.,-1.));
#7938=DIRECTION('center_axis',(0.866025403784439,0.,-0.5));
#7939=DIRECTION('ref_axis',(0.5,0.,0.866025403784439));
#7940=DIRECTION('',(-0.5,0.,-0.866025403784439));
#7941=DIRECTION('',(0.,-1.,0.));
#7942=DIRECTION('',(0.5,0.,0.866025403784439));
#7943=DIRECTION('',(0.,-1.,0.));
#7944=DIRECTION('center_axis',(1.60246890531964E-16,0.,-1.));
#7945=DIRECTION('ref_axis',(1.,0.,1.60246890531964E-16));
#7946=DIRECTION('',(-1.,0.,-1.60246890531964E-16));
#7947=DIRECTION('',(0.,-1.,0.));
#7948=DIRECTION('',(1.,0.,1.60246890531964E-16));
#7949=DIRECTION('center_axis',(-0.866025403784439,0.,-0.5));
#7950=DIRECTION('ref_axis',(0.5,0.,-0.866025403784439));
#7951=DIRECTION('',(-0.5,0.,0.866025403784439));
#7952=DIRECTION('',(0.,-1.,0.));
#7953=DIRECTION('',(0.5,0.,-0.866025403784439));
#7954=DIRECTION('center_axis',(-0.866025403784439,0.,0.5));
#7955=DIRECTION('ref_axis',(-0.5,0.,-0.866025403784439));
#7956=DIRECTION('',(0.5,0.,0.866025403784439));
#7957=DIRECTION('',(0.,-1.,0.));
#7958=DIRECTION('',(-0.5,0.,-0.866025403784439));
#7959=DIRECTION('center_axis',(-1.60246890531964E-16,0.,1.));
#7960=DIRECTION('ref_axis',(-1.,0.,-1.60246890531964E-16));
#7961=DIRECTION('',(1.,0.,1.60246890531964E-16));
#7962=DIRECTION('',(0.,-1.,0.));
#7963=DIRECTION('',(-1.,0.,-1.60246890531964E-16));
#7964=DIRECTION('center_axis',(0.866025403784439,0.,0.5));
#7965=DIRECTION('ref_axis',(-0.5,0.,0.866025403784439));
#7966=DIRECTION('',(0.5,0.,-0.866025403784439));
#7967=DIRECTION('',(-0.5,0.,0.866025403784439));
#7968=DIRECTION('center_axis',(0.,1.,0.));
#7969=DIRECTION('ref_axis',(1.,0.,0.));
#7970=DIRECTION('center_axis',(0.,-1.,0.));
#7971=DIRECTION('ref_axis',(0.,0.,-1.));
#7972=DIRECTION('axis',(0.,0.,1.));
#7973=DIRECTION('refdir',(1.,0.,0.));
#7974=DIRECTION('center_axis',(0.,1.,0.));
#7975=DIRECTION('ref_axis',(1.,0.,0.));
#7976=DIRECTION('center_axis',(0.,-1.,0.));
#7977=DIRECTION('ref_axis',(1.,0.,0.));
#7978=DIRECTION('',(0.,-1.,0.));
#7979=DIRECTION('center_axis',(0.,-1.,0.));
#7980=DIRECTION('ref_axis',(1.,0.,0.));
#7981=DIRECTION('center_axis',(0.,1.,0.));
#7982=DIRECTION('ref_axis',(1.,0.,0.));
#7983=DIRECTION('center_axis',(0.,1.,0.));
#7984=DIRECTION('ref_axis',(1.,0.,0.));
#7985=DIRECTION('',(0.,-1.,0.));
#7986=DIRECTION('center_axis',(0.,1.,0.));
#7987=DIRECTION('ref_axis',(1.,0.,0.));
#7988=DIRECTION('center_axis',(0.,1.,0.));
#7989=DIRECTION('ref_axis',(1.,0.,0.));
#7990=DIRECTION('center_axis',(0.,1.,0.));
#7991=DIRECTION('ref_axis',(1.,0.,0.));
#7992=DIRECTION('axis',(0.,0.,1.));
#7993=DIRECTION('refdir',(1.,0.,0.));
#7994=DIRECTION('center_axis',(0.,1.,0.));
#7995=DIRECTION('ref_axis',(1.,0.,0.));
#7996=DIRECTION('',(0.866025403784439,-0.5,1.06057523872491E-16));
#7997=DIRECTION('center_axis',(0.,-1.,0.));
#7998=DIRECTION('ref_axis',(1.,0.,0.));
#7999=DIRECTION('center_axis',(0.,-1.,0.));
#8000=DIRECTION('ref_axis',(1.,0.,0.));
#8001=DIRECTION('center_axis',(0.,1.,0.));
#8002=DIRECTION('ref_axis',(1.,0.,0.));
#8003=DIRECTION('',(-0.866025403784439,-0.5,-1.06057523872491E-16));
#8004=DIRECTION('center_axis',(1.4792020664489E-16,0.,-1.));
#8005=DIRECTION('ref_axis',(-1.,0.,-1.4792020664489E-16));
#8006=DIRECTION('',(0.,1.,0.));
#8007=DIRECTION('',(0.,1.,0.));
#8008=DIRECTION('center_axis',(-0.866025403784439,0.,-0.5));
#8009=DIRECTION('ref_axis',(-0.5,0.,0.866025403784439));
#8010=DIRECTION('',(0.,1.,0.));
#8011=DIRECTION('center_axis',(-0.866025403784439,0.,0.5));
#8012=DIRECTION('ref_axis',(0.5,0.,0.866025403784439));
#8013=DIRECTION('',(0.,1.,0.));
#8014=DIRECTION('center_axis',(0.,1.,0.));
#8015=DIRECTION('ref_axis',(1.,0.,0.));
#8016=DIRECTION('center_axis',(0.,1.,0.));
#8017=DIRECTION('ref_axis',(1.,0.,0.));
#8018=DIRECTION('',(0.,-1.,0.));
#8019=DIRECTION('center_axis',(0.,1.,0.));
#8020=DIRECTION('ref_axis',(1.,0.,0.));
#8021=DIRECTION('center_axis',(-2.95840413289779E-16,0.,1.));
#8022=DIRECTION('ref_axis',(1.,0.,2.95840413289779E-16));
#8023=DIRECTION('',(0.,1.,0.));
#8024=DIRECTION('center_axis',(0.866025403784439,0.,-0.5));
#8025=DIRECTION('ref_axis',(-0.5,0.,-0.866025403784439));
#8026=DIRECTION('',(0.,1.,0.));
#8027=DIRECTION('center_axis',(0.866025403784439,0.,0.5));
#8028=DIRECTION('ref_axis',(0.5,0.,-0.866025403784439));
#8029=DIRECTION('center_axis',(0.,1.,0.));
#8030=DIRECTION('ref_axis',(1.,0.,0.));
#8031=DIRECTION('center_axis',(0.,1.,0.));
#8032=DIRECTION('ref_axis',(1.,0.,0.));
#8033=DIRECTION('',(0.,0.,1.));
#8034=DIRECTION('',(2.22044604925031E-16,1.,0.));
#8035=DIRECTION('',(0.,0.,1.));
#8036=DIRECTION('',(1.,0.,0.));
#8037=DIRECTION('',(0.,0.,1.));
#8038=DIRECTION('',(1.,0.,0.));
#8039=DIRECTION('',(0.,0.,1.));
#8040=DIRECTION('',(1.,0.,0.));
#8041=DIRECTION('',(0.,0.,1.));
#8042=DIRECTION('',(1.,0.,0.));
#8043=DIRECTION('',(0.,0.,1.));
#8044=DIRECTION('',(1.,0.,0.));
#8045=DIRECTION('',(0.,0.,1.));
#8046=DIRECTION('',(1.,0.,0.));
#8047=DIRECTION('',(0.,0.,1.));
#8048=DIRECTION('',(-1.,1.22464679914735E-16,0.));
#8049=DIRECTION('',(0.,0.,1.));
#8050=DIRECTION('',(1.,0.,0.));
#8051=DIRECTION('',(0.,0.,1.));
#8052=DIRECTION('',(-1.,1.22464679914735E-16,0.));
#8053=DIRECTION('',(0.,0.,1.));
#8054=DIRECTION('',(1.,0.,0.));
#8055=DIRECTION('',(0.,0.,1.));
#8056=DIRECTION('',(2.22044604925031E-16,1.,0.));
#8057=DIRECTION('',(0.,0.,1.));
#8058=DIRECTION('',(2.22044604925031E-16,-1.,0.));
#8059=DIRECTION('',(0.,0.,1.));
#8060=DIRECTION('',(2.22044604925031E-16,-1.,0.));
#8061=DIRECTION('',(0.,0.,1.));
#8062=DIRECTION('',(1.,0.,0.));
#8063=DIRECTION('',(0.,0.,1.));
#8064=DIRECTION('',(1.,0.,0.));
#8065=DIRECTION('',(0.,0.,1.));
#8066=DIRECTION('',(2.22044604925031E-16,-1.,0.));
#8067=DIRECTION('',(0.,0.,1.));
#8068=DIRECTION('',(2.22044604925031E-16,1.,0.));
#8069=DIRECTION('',(0.,0.,1.));
#8070=DIRECTION('',(2.22044604925031E-16,-1.,0.));
#8071=DIRECTION('',(0.,0.,1.));
#8072=DIRECTION('',(2.22044604925031E-16,-1.,0.));
#8073=DIRECTION('',(0.,0.,1.));
#8074=DIRECTION('',(2.22044604925031E-16,-1.,0.));
#8075=DIRECTION('',(0.,0.,1.));
#8076=DIRECTION('',(2.22044604925031E-16,1.,0.));
#8077=DIRECTION('',(0.,0.,1.));
#8078=DIRECTION('',(2.22044604925031E-16,-1.,0.));
#8079=DIRECTION('',(0.,0.,1.));
#8080=DIRECTION('',(2.22044604925031E-16,-1.,0.));
#8081=DIRECTION('',(0.,0.,1.));
#8082=DIRECTION('',(2.22044604925031E-16,-1.,0.));
#8083=DIRECTION('',(0.,0.,1.));
#8084=DIRECTION('',(2.22044604925031E-16,1.,0.));
#8085=DIRECTION('',(0.,0.,1.));
#8086=DIRECTION('',(2.22044604925031E-16,-1.,0.));
#8087=DIRECTION('',(0.,0.,1.));
#8088=DIRECTION('',(2.22044604925031E-16,-1.,0.));
#8089=DIRECTION('',(0.,0.,1.));
#8090=DIRECTION('',(2.22044604925031E-16,-1.,0.));
#8091=DIRECTION('',(0.,0.,1.));
#8092=DIRECTION('',(2.22044604925031E-16,1.,0.));
#8093=DIRECTION('',(0.,0.,1.));
#8094=DIRECTION('',(2.22044604925031E-16,-1.,0.));
#8095=DIRECTION('',(0.,0.,1.));
#8096=DIRECTION('',(2.22044604925031E-16,-1.,0.));
#8097=DIRECTION('axis',(0.,0.,1.));
#8098=DIRECTION('refdir',(1.,0.,0.));
#8099=DIRECTION('axis',(0.,0.,1.));
#8100=DIRECTION('refdir',(1.,0.,0.));
#8101=DIRECTION('center_axis',(0.,-1.,0.));
#8102=DIRECTION('ref_axis',(1.,0.,0.));
#8103=DIRECTION('center_axis',(0.,-1.,0.));
#8104=DIRECTION('ref_axis',(0.,0.,1.));
#8105=DIRECTION('',(0.,0.,1.));
#8106=DIRECTION('',(1.,0.,0.));
#8107=DIRECTION('',(0.,0.,1.));
#8108=DIRECTION('center_axis',(-1.,0.,0.));
#8109=DIRECTION('ref_axis',(0.,-1.,0.));
#8110=DIRECTION('center_axis',(-1.,0.,0.));
#8111=DIRECTION('ref_axis',(0.,0.,-1.));
#8112=DIRECTION('',(0.,-1.,0.));
#8113=DIRECTION('',(0.,0.,1.));
#8114=DIRECTION('center_axis',(-1.,0.,0.));
#8115=DIRECTION('ref_axis',(0.,0.,-1.));
#8116=DIRECTION('center_axis',(0.,1.,0.));
#8117=DIRECTION('ref_axis',(-1.,0.,0.));
#8118=DIRECTION('center_axis',(0.,1.,0.));
#8119=DIRECTION('ref_axis',(0.,0.,-1.));
#8120=DIRECTION('',(-1.,0.,0.));
#8121=DIRECTION('',(0.,0.,1.));
#8122=DIRECTION('center_axis',(1.,0.,0.));
#8123=DIRECTION('ref_axis',(0.,1.,0.));
#8124=DIRECTION('center_axis',(1.,0.,0.));
#8125=DIRECTION('ref_axis',(0.,0.,1.));
#8126=DIRECTION('',(0.,1.,0.));
#8127=DIRECTION('center_axis',(0.,0.,1.));
#8128=DIRECTION('ref_axis',(1.,0.,0.));
#8129=DIRECTION('center_axis',(0.,1.,0.));
#8130=DIRECTION('ref_axis',(1.,0.,0.));
#8131=DIRECTION('center_axis',(0.,1.,0.));
#8132=DIRECTION('ref_axis',(1.,0.,0.));
#8133=DIRECTION('',(0.,1.,0.));
#8134=DIRECTION('center_axis',(0.,-1.,0.));
#8135=DIRECTION('ref_axis',(1.,0.,0.));
#8136=DIRECTION('center_axis',(6.12323399573677E-17,0.,1.));
#8137=DIRECTION('ref_axis',(1.,0.,0.));
#8138=DIRECTION('center_axis',(1.22464679914735E-16,-1.,0.));
#8139=DIRECTION('ref_axis',(-1.,-1.22464679914735E-16,0.));
#8140=DIRECTION('axis',(0.,0.,1.));
#8141=DIRECTION('refdir',(1.,0.,0.));
#8142=DIRECTION('center_axis',(0.,0.,1.));
#8143=DIRECTION('ref_axis',(1.,0.,0.));
#8144=DIRECTION('center_axis',(0.,0.,1.));
#8145=DIRECTION('ref_axis',(1.,0.,0.));
#8146=DIRECTION('',(0.,0.,1.));
#8147=DIRECTION('center_axis',(0.,0.,-1.));
#8148=DIRECTION('ref_axis',(1.,0.,0.));
#8149=DIRECTION('center_axis',(0.,0.,1.));
#8150=DIRECTION('ref_axis',(1.,0.,0.));
#8151=DIRECTION('center_axis',(0.,0.,1.));
#8152=DIRECTION('ref_axis',(1.,0.,0.));
#8153=DIRECTION('center_axis',(0.,0.,1.));
#8154=DIRECTION('ref_axis',(1.,0.,0.));
#8155=DIRECTION('',(0.,-1.,0.));
#8156=DIRECTION('',(-1.,0.,0.));
#8157=DIRECTION('center_axis',(0.,0.,1.));
#8158=DIRECTION('ref_axis',(1.,0.,0.));
#8159=DIRECTION('center_axis',(0.,0.,1.));
#8160=DIRECTION('ref_axis',(1.,0.,0.));
#8161=DIRECTION('',(1.,0.,0.));
#8162=DIRECTION('',(0.,-1.,0.));
#8163=DIRECTION('center_axis',(0.,0.,1.));
#8164=DIRECTION('ref_axis',(1.,0.,0.));
#8165=DIRECTION('center_axis',(0.,0.,1.));
#8166=DIRECTION('ref_axis',(1.,0.,0.));
#8167=DIRECTION('',(0.,1.,0.));
#8168=DIRECTION('',(1.,0.,0.));
#8169=DIRECTION('center_axis',(0.,0.,1.));
#8170=DIRECTION('ref_axis',(1.,0.,0.));
#8171=DIRECTION('center_axis',(0.,0.,1.));
#8172=DIRECTION('ref_axis',(1.,0.,0.));
#8173=DIRECTION('',(-1.,0.,0.));
#8174=DIRECTION('',(0.,1.,0.));
#8175=DIRECTION('center_axis',(0.,1.,0.));
#8176=DIRECTION('ref_axis',(-1.,0.,0.));
#8177=DIRECTION('',(1.,0.,0.));
#8178=DIRECTION('',(0.,0.,1.));
#8179=DIRECTION('',(-1.,0.,0.));
#8180=DIRECTION('',(0.,0.,1.));
#8181=DIRECTION('center_axis',(1.,0.,0.));
#8182=DIRECTION('ref_axis',(0.,1.,0.));
#8183=DIRECTION('',(0.,-1.,0.));
#8184=DIRECTION('',(0.,1.,0.));
#8185=DIRECTION('',(0.,0.,1.));
#8186=DIRECTION('center_axis',(0.,-1.,0.));
#8187=DIRECTION('ref_axis',(1.,0.,0.));
#8188=DIRECTION('',(-1.,0.,0.));
#8189=DIRECTION('',(1.,0.,0.));
#8190=DIRECTION('',(0.,0.,1.));
#8191=DIRECTION('center_axis',(-1.,0.,0.));
#8192=DIRECTION('ref_axis',(0.,-1.,0.));
#8193=DIRECTION('',(0.,1.,0.));
#8194=DIRECTION('',(0.,-1.,0.));
#8195=DIRECTION('center_axis',(0.,0.,1.));
#8196=DIRECTION('ref_axis',(1.,0.,0.));
#8197=DIRECTION('center_axis',(0.,0.,1.));
#8198=DIRECTION('ref_axis',(1.,0.,0.));
#8199=DIRECTION('center_axis',(0.,0.,1.));
#8200=DIRECTION('ref_axis',(1.,0.,0.));
#8201=DIRECTION('center_axis',(0.,0.,1.));
#8202=DIRECTION('ref_axis',(1.,0.,0.));
#8203=DIRECTION('center_axis',(0.,0.,1.));
#8204=DIRECTION('ref_axis',(1.,0.,0.));
#8205=DIRECTION('center_axis',(0.,0.,1.));
#8206=DIRECTION('ref_axis',(1.,0.,0.));
#8207=DIRECTION('center_axis',(0.,0.,1.));
#8208=DIRECTION('ref_axis',(1.,0.,0.));
#8209=DIRECTION('center_axis',(0.,0.,1.));
#8210=DIRECTION('ref_axis',(1.,0.,0.));
#8211=DIRECTION('center_axis',(0.,0.,1.));
#8212=DIRECTION('ref_axis',(1.,0.,0.));
#8213=DIRECTION('center_axis',(0.,0.,1.));
#8214=DIRECTION('ref_axis',(1.,0.,0.));
#8215=DIRECTION('center_axis',(0.,1.,0.));
#8216=DIRECTION('ref_axis',(-1.,0.,0.));
#8217=DIRECTION('',(-1.,0.,0.));
#8218=DIRECTION('',(0.,0.,1.));
#8219=DIRECTION('',(-1.,0.,0.));
#8220=DIRECTION('',(0.,0.,1.));
#8221=DIRECTION('center_axis',(1.,0.,0.));
#8222=DIRECTION('ref_axis',(0.,1.,0.));
#8223=DIRECTION('',(0.,1.,0.));
#8224=DIRECTION('',(0.,1.,0.));
#8225=DIRECTION('',(0.,0.,1.));
#8226=DIRECTION('center_axis',(0.,-1.,0.));
#8227=DIRECTION('ref_axis',(1.,0.,0.));
#8228=DIRECTION('',(1.,0.,0.));
#8229=DIRECTION('',(1.,0.,0.));
#8230=DIRECTION('',(0.,0.,1.));
#8231=DIRECTION('center_axis',(-1.,0.,0.));
#8232=DIRECTION('ref_axis',(0.,-1.,0.));
#8233=DIRECTION('',(0.,-1.,0.));
#8234=DIRECTION('',(0.,-1.,0.));
#8235=DIRECTION('center_axis',(0.,0.,1.));
#8236=DIRECTION('ref_axis',(1.,0.,0.));
#8237=DIRECTION('center_axis',(0.,0.,1.));
#8238=DIRECTION('ref_axis',(1.,0.,0.));
#8239=DIRECTION('',(0.,0.,-1.));
#8240=DIRECTION('center_axis',(0.,0.,1.));
#8241=DIRECTION('ref_axis',(1.,0.,0.));
#8242=DIRECTION('center_axis',(0.,0.,1.));
#8243=DIRECTION('ref_axis',(1.,0.,0.));
#8244=DIRECTION('axis',(0.,0.,1.));
#8245=DIRECTION('refdir',(1.,0.,0.));
#8246=DIRECTION('center_axis',(0.,-1.,0.));
#8247=DIRECTION('ref_axis',(1.,0.,0.));
#8248=DIRECTION('',(-1.,0.,0.));
#8249=DIRECTION('',(0.,0.,1.));
#8250=DIRECTION('',(1.,0.,0.));
#8251=DIRECTION('',(0.,0.,1.));
#8252=DIRECTION('center_axis',(-1.,0.,0.));
#8253=DIRECTION('ref_axis',(0.,-1.,0.));
#8254=DIRECTION('',(0.,1.,0.));
#8255=DIRECTION('',(0.,-1.,0.));
#8256=DIRECTION('',(0.,0.,1.));
#8257=DIRECTION('center_axis',(0.,1.,0.));
#8258=DIRECTION('ref_axis',(-1.,0.,0.));
#8259=DIRECTION('',(1.,0.,0.));
#8260=DIRECTION('',(-1.,0.,0.));
#8261=DIRECTION('',(0.,0.,1.));
#8262=DIRECTION('center_axis',(1.,0.,0.));
#8263=DIRECTION('ref_axis',(0.,1.,0.));
#8264=DIRECTION('',(0.,-1.,0.));
#8265=DIRECTION('',(0.,1.,0.));
#8266=DIRECTION('center_axis',(0.,1.,0.));
#8267=DIRECTION('ref_axis',(-1.,0.,0.));
#8268=DIRECTION('',(-1.,0.,0.));
#8269=DIRECTION('',(0.,0.,1.));
#8270=DIRECTION('',(-1.,0.,0.));
#8271=DIRECTION('',(0.,0.,1.));
#8272=DIRECTION('center_axis',(1.,0.,0.));
#8273=DIRECTION('ref_axis',(0.,1.,0.));
#8274=DIRECTION('',(0.,1.,0.));
#8275=DIRECTION('',(0.,1.,0.));
#8276=DIRECTION('',(0.,0.,1.));
#8277=DIRECTION('center_axis',(0.,-1.,0.));
#8278=DIRECTION('ref_axis',(1.,0.,0.));
#8279=DIRECTION('',(1.,0.,0.));
#8280=DIRECTION('',(1.,0.,0.));
#8281=DIRECTION('',(0.,0.,1.));
#8282=DIRECTION('center_axis',(-1.,0.,0.));
#8283=DIRECTION('ref_axis',(0.,-1.,0.));
#8284=DIRECTION('',(0.,-1.,0.));
#8285=DIRECTION('',(0.,-1.,0.));
#8286=DIRECTION('center_axis',(0.,0.,1.));
#8287=DIRECTION('ref_axis',(1.,0.,0.));
#8288=DIRECTION('center_axis',(0.,0.,1.));
#8289=DIRECTION('ref_axis',(1.,0.,0.));
#8290=DIRECTION('axis',(0.,0.,1.));
#8291=DIRECTION('refdir',(1.,0.,0.));
#8292=DIRECTION('center_axis',(0.,0.,1.));
#8293=DIRECTION('ref_axis',(1.,0.,0.));
#8294=DIRECTION('center_axis',(0.,0.,-1.));
#8295=DIRECTION('ref_axis',(1.,0.,0.));
#8296=DIRECTION('',(0.,0.,-1.));
#8297=DIRECTION('center_axis',(0.,0.,-1.));
#8298=DIRECTION('ref_axis',(1.,0.,0.));
#8299=DIRECTION('center_axis',(0.,0.,1.));
#8300=DIRECTION('ref_axis',(1.,0.,0.));
#8301=DIRECTION('center_axis',(0.,0.,1.));
#8302=DIRECTION('ref_axis',(1.,0.,0.));
#8303=DIRECTION('',(0.,0.,-1.));
#8304=DIRECTION('center_axis',(0.,0.,1.));
#8305=DIRECTION('ref_axis',(1.,0.,0.));
#8306=DIRECTION('center_axis',(0.,0.,1.));
#8307=DIRECTION('ref_axis',(1.,0.,0.));
#8308=DIRECTION('center_axis',(0.,0.,1.));
#8309=DIRECTION('ref_axis',(1.,0.,0.));
#8310=DIRECTION('axis',(0.,0.,1.));
#8311=DIRECTION('refdir',(1.,0.,0.));
#8312=DIRECTION('center_axis',(0.,1.,0.));
#8313=DIRECTION('ref_axis',(-1.,0.,0.));
#8314=DIRECTION('',(-1.,0.,0.));
#8315=DIRECTION('',(0.,0.,1.));
#8316=DIRECTION('',(-1.,0.,0.));
#8317=DIRECTION('',(0.,0.,1.));
#8318=DIRECTION('center_axis',(1.,0.,0.));
#8319=DIRECTION('ref_axis',(0.,1.,0.));
#8320=DIRECTION('',(0.,1.,0.));
#8321=DIRECTION('',(0.,1.,0.));
#8322=DIRECTION('',(0.,0.,1.));
#8323=DIRECTION('center_axis',(0.,-1.,0.));
#8324=DIRECTION('ref_axis',(1.,0.,0.));
#8325=DIRECTION('',(1.,0.,0.));
#8326=DIRECTION('',(1.,0.,0.));
#8327=DIRECTION('',(0.,0.,1.));
#8328=DIRECTION('center_axis',(-1.,0.,0.));
#8329=DIRECTION('ref_axis',(0.,-1.,0.));
#8330=DIRECTION('',(0.,-1.,0.));
#8331=DIRECTION('',(0.,-1.,0.));
#8332=DIRECTION('center_axis',(0.,0.,1.));
#8333=DIRECTION('ref_axis',(1.,0.,0.));
#8334=DIRECTION('center_axis',(0.,0.,1.));
#8335=DIRECTION('ref_axis',(1.,0.,0.));
#8336=DIRECTION('axis',(0.,0.,1.));
#8337=DIRECTION('refdir',(1.,0.,0.));
#8338=DIRECTION('center_axis',(0.866025403784439,0.,-0.5));
#8339=DIRECTION('ref_axis',(0.5,0.,0.866025403784439));
#8340=DIRECTION('',(-0.5,0.,-0.866025403784439));
#8341=DIRECTION('',(0.,-1.,0.));
#8342=DIRECTION('',(0.5,0.,0.866025403784439));
#8343=DIRECTION('',(0.,-1.,0.));
#8344=DIRECTION('center_axis',(1.60246890531964E-16,0.,-1.));
#8345=DIRECTION('ref_axis',(1.,0.,1.60246890531964E-16));
#8346=DIRECTION('',(-1.,0.,-1.60246890531964E-16));
#8347=DIRECTION('',(0.,-1.,0.));
#8348=DIRECTION('',(1.,0.,1.60246890531964E-16));
#8349=DIRECTION('center_axis',(-0.866025403784439,0.,-0.5));
#8350=DIRECTION('ref_axis',(0.5,0.,-0.866025403784439));
#8351=DIRECTION('',(-0.5,0.,0.866025403784439));
#8352=DIRECTION('',(0.,-1.,0.));
#8353=DIRECTION('',(0.5,0.,-0.866025403784439));
#8354=DIRECTION('center_axis',(-0.866025403784439,0.,0.5));
#8355=DIRECTION('ref_axis',(-0.5,0.,-0.866025403784439));
#8356=DIRECTION('',(0.5,0.,0.866025403784439));
#8357=DIRECTION('',(0.,-1.,0.));
#8358=DIRECTION('',(-0.5,0.,-0.866025403784439));
#8359=DIRECTION('center_axis',(-1.60246890531964E-16,0.,1.));
#8360=DIRECTION('ref_axis',(-1.,0.,-1.60246890531964E-16));
#8361=DIRECTION('',(1.,0.,1.60246890531964E-16));
#8362=DIRECTION('',(0.,-1.,0.));
#8363=DIRECTION('',(-1.,0.,-1.60246890531964E-16));
#8364=DIRECTION('center_axis',(0.866025403784439,0.,0.5));
#8365=DIRECTION('ref_axis',(-0.5,0.,0.866025403784439));
#8366=DIRECTION('',(0.5,0.,-0.866025403784439));
#8367=DIRECTION('',(-0.5,0.,0.866025403784439));
#8368=DIRECTION('center_axis',(0.,1.,0.));
#8369=DIRECTION('ref_axis',(1.,0.,0.));
#8370=DIRECTION('center_axis',(0.,-1.,0.));
#8371=DIRECTION('ref_axis',(0.,0.,-1.));
#8372=DIRECTION('center_axis',(0.,1.,0.));
#8373=DIRECTION('ref_axis',(1.,0.,0.));
#8374=DIRECTION('center_axis',(0.,1.,0.));
#8375=DIRECTION('ref_axis',(1.,0.,0.));
#8376=DIRECTION('center_axis',(0.,1.,0.));
#8377=DIRECTION('ref_axis',(0.,0.,1.));
#8378=DIRECTION('center_axis',(0.,-1.,0.));
#8379=DIRECTION('ref_axis',(1.,0.,0.));
#8380=DIRECTION('center_axis',(0.,-1.,0.));
#8381=DIRECTION('ref_axis',(1.,0.,0.));
#8382=DIRECTION('center_axis',(0.,-1.,0.));
#8383=DIRECTION('ref_axis',(1.,0.,0.));
#8384=DIRECTION('',(0.707106781186547,0.707106781186548,8.65956056235493E-17));
#8385=DIRECTION('center_axis',(0.,-1.,0.));
#8386=DIRECTION('ref_axis',(1.,0.,0.));
#8387=DIRECTION('center_axis',(0.,-1.,0.));
#8388=DIRECTION('ref_axis',(1.,0.,0.));
#8389=DIRECTION('',(0.,1.,0.));
#8390=DIRECTION('center_axis',(0.,1.,0.));
#8391=DIRECTION('ref_axis',(1.,0.,0.));
#8392=DIRECTION('center_axis',(0.,-1.,0.));
#8393=DIRECTION('ref_axis',(1.,0.,0.));
#8394=DIRECTION('',(-0.707106781186547,0.707106781186548,-8.65956056235493E-17));
#8395=DIRECTION('center_axis',(0.,-1.,0.));
#8396=DIRECTION('ref_axis',(0.,0.,-1.));
#8397=DIRECTION('center_axis',(0.,-1.,0.));
#8398=DIRECTION('ref_axis',(1.,0.,0.));
#8399=DIRECTION('center_axis',(0.,1.,0.));
#8400=DIRECTION('ref_axis',(1.,0.,0.));
#8401=DIRECTION('center_axis',(0.,1.,0.));
#8402=DIRECTION('ref_axis',(1.,0.,0.));
#8403=DIRECTION('',(-0.447213595499958,0.894427190999916,-5.47678698264203E-17));
#8404=DIRECTION('center_axis',(0.,-1.,0.));
#8405=DIRECTION('ref_axis',(1.,0.,0.));
#8406=DIRECTION('',(0.,1.,0.));
#8407=DIRECTION('',(0.,0.,1.));
#8408=DIRECTION('',(1.,0.,0.));
#8409=DIRECTION('',(0.,0.,1.));
#8410=DIRECTION('',(1.,0.,0.));
#8411=DIRECTION('',(0.,0.,1.));
#8412=DIRECTION('',(1.,0.,0.));
#8413=DIRECTION('',(0.,0.,1.));
#8414=DIRECTION('',(1.,0.,0.));
#8415=DIRECTION('',(0.,0.,1.));
#8416=DIRECTION('',(1.,0.,0.));
#8417=DIRECTION('',(0.,-1.,2.22044604925031E-16));
#8418=DIRECTION('',(1.,0.,0.));
#8419=DIRECTION('',(0.,0.,1.));
#8420=DIRECTION('',(1.,0.,0.));
#8421=DIRECTION('',(0.,0.,1.));
#8422=DIRECTION('',(2.22044604925031E-16,1.,0.));
#8423=CARTESIAN_POINT('',(0.,0.,0.));
#8424=CARTESIAN_POINT('',(0.,0.,0.));
#8425=CARTESIAN_POINT('',(0.,0.,0.));
#8426=CARTESIAN_POINT('',(0.,0.,0.));
#8427=CARTESIAN_POINT('Origin',(-1.3,-1.,6.8));
#8428=CARTESIAN_POINT('',(-1.465,-1.,6.8));
#8429=CARTESIAN_POINT('Origin',(-1.3,-1.,6.8));
#8430=CARTESIAN_POINT('',(-1.465,-1.,7.5));
#8431=CARTESIAN_POINT('',(-1.465,-1.,6.8));
#8432=CARTESIAN_POINT('Origin',(-1.3,-1.,7.5));
#8433=CARTESIAN_POINT('Origin',(-1.3,-1.,6.8));
#8434=CARTESIAN_POINT('Origin',(1.3,-1.,6.8));
#8435=CARTESIAN_POINT('',(1.135,-1.,6.8));
#8436=CARTESIAN_POINT('Origin',(1.3,-1.,6.8));
#8437=CARTESIAN_POINT('',(1.135,-1.,7.5));
#8438=CARTESIAN_POINT('',(1.135,-1.,6.8));
#8439=CARTESIAN_POINT('Origin',(1.3,-1.,7.5));
#8440=CARTESIAN_POINT('Origin',(1.3,-1.,6.8));
#8441=CARTESIAN_POINT('Origin',(1.9,-3.1,3.1));
#8442=CARTESIAN_POINT('',(1.625,-3.,3.1));
#8443=CARTESIAN_POINT('Origin',(1.9,-3.,3.1));
#8444=CARTESIAN_POINT('',(1.625,-0.0249999999999999,3.1));
#8445=CARTESIAN_POINT('',(1.625,-3.1,3.1));
#8446=CARTESIAN_POINT('Origin',(1.9,-0.0249999999999999,3.1));
#8447=CARTESIAN_POINT('Origin',(-1.9,-3.1,6.9));
#8448=CARTESIAN_POINT('',(-2.175,-3.,6.9));
#8449=CARTESIAN_POINT('Origin',(-1.9,-3.,6.9));
#8450=CARTESIAN_POINT('',(-2.175,-0.0249999999999999,6.9));
#8451=CARTESIAN_POINT('',(-2.175,-3.1,6.9));
#8452=CARTESIAN_POINT('Origin',(-1.9,-0.0249999999999999,6.9));
#8453=CARTESIAN_POINT('Origin',(-1.9,-3.1,3.1));
#8454=CARTESIAN_POINT('',(-2.175,-3.,3.1));
#8455=CARTESIAN_POINT('Origin',(-1.9,-3.,3.1));
#8456=CARTESIAN_POINT('',(-2.175,-0.0249999999999999,3.1));
#8457=CARTESIAN_POINT('',(-2.175,-3.1,3.1));
#8458=CARTESIAN_POINT('Origin',(-1.9,-0.0249999999999999,3.1));
#8459=CARTESIAN_POINT('Origin',(1.9,-3.1,6.9));
#8460=CARTESIAN_POINT('',(1.625,-3.,6.9));
#8461=CARTESIAN_POINT('Origin',(1.9,-3.,6.9));
#8462=CARTESIAN_POINT('',(1.625,-0.0249999999999999,6.9));
#8463=CARTESIAN_POINT('',(1.625,-3.1,6.9));
#8464=CARTESIAN_POINT('Origin',(1.9,-0.0249999999999999,6.9));
#8465=CARTESIAN_POINT('Origin',(0.,0.,6.5));
#8466=CARTESIAN_POINT('',(0.699553428981661,-0.025,6.5));
#8467=CARTESIAN_POINT('',(0.699553428981661,-0.025,7.5));
#8468=CARTESIAN_POINT('',(0.699553428981661,-0.025,6.5));
#8469=CARTESIAN_POINT('',(-0.699553428981661,-0.025,6.5));
#8470=CARTESIAN_POINT('Origin',(0.,0.,6.5));
#8471=CARTESIAN_POINT('',(-0.699553428981661,-0.025,7.5));
#8472=CARTESIAN_POINT('',(-0.699553428981661,-0.025,6.5));
#8473=CARTESIAN_POINT('Origin',(0.,0.,7.5));
#8474=CARTESIAN_POINT('Origin',(0.,0.,6.5));
#8475=CARTESIAN_POINT('',(0.556214886532175,-0.025,6.5));
#8476=CARTESIAN_POINT('',(1.25,-0.025,6.5));
#8477=CARTESIAN_POINT('',(-0.556214886532175,-0.025,6.5));
#8478=CARTESIAN_POINT('Origin',(0.,0.,6.5));
#8479=CARTESIAN_POINT('',(1.25,-0.025,6.5));
#8480=CARTESIAN_POINT('Origin',(0.,-1.5125,7.5));
#8481=CARTESIAN_POINT('',(-2.5,-0.025,7.5));
#8482=CARTESIAN_POINT('',(2.5,-0.025,7.5));
#8483=CARTESIAN_POINT('',(-2.5,-3.,7.5));
#8484=CARTESIAN_POINT('',(-2.5,-0.025,7.5));
#8485=CARTESIAN_POINT('',(2.5,-3.,7.5));
#8486=CARTESIAN_POINT('',(-2.5,-3.,7.5));
#8487=CARTESIAN_POINT('',(2.5,-0.025,7.5));
#8488=CARTESIAN_POINT('',(2.5,-3.,7.5));
#8489=CARTESIAN_POINT('',(2.5,-0.025,7.5));
#8490=CARTESIAN_POINT('Origin',(0.,-3.1,5.));
#8491=CARTESIAN_POINT('',(-0.93,-3.,5.));
#8492=CARTESIAN_POINT('Origin',(0.,-3.,5.));
#8493=CARTESIAN_POINT('',(-0.93,-1.8,5.));
#8494=CARTESIAN_POINT('',(-0.93,-3.1,5.));
#8495=CARTESIAN_POINT('Origin',(0.,-1.8,5.));
#8496=CARTESIAN_POINT('Origin',(0.,-1.8,5.));
#8497=CARTESIAN_POINT('',(-1.3,-1.8,5.));
#8498=CARTESIAN_POINT('Origin',(0.,-1.8,5.));
#8499=CARTESIAN_POINT('',(-1.3,-1.,5.));
#8500=CARTESIAN_POINT('',(-1.3,-1.8,5.));
#8501=CARTESIAN_POINT('Origin',(0.,-1.,5.));
#8502=CARTESIAN_POINT('Origin',(0.,-1.,5.));
#8503=CARTESIAN_POINT('',(-1.52958336188405E-16,-1.,6.24899959967968));
#8504=CARTESIAN_POINT('Origin',(0.,-1.,5.));
#8505=CARTESIAN_POINT('Origin',(0.,-1.8,5.));
#8506=CARTESIAN_POINT('Origin',(0.,0.,5.));
#8507=CARTESIAN_POINT('Origin',(0.,-0.025,5.));
#8508=CARTESIAN_POINT('Origin',(2.5,-0.025,2.5));
#8509=CARTESIAN_POINT('',(2.5,-0.025,2.5));
#8510=CARTESIAN_POINT('',(2.5,-0.025,2.5));
#8511=CARTESIAN_POINT('',(-2.5,-0.025,2.5));
#8512=CARTESIAN_POINT('',(2.5,-0.025,2.5));
#8513=CARTESIAN_POINT('',(-2.5,-0.025,2.5));
#8514=CARTESIAN_POINT('Origin',(2.5,-3.,2.5));
#8515=CARTESIAN_POINT('',(2.5,-3.,2.5));
#8516=CARTESIAN_POINT('',(2.5,-3.,2.5));
#8517=CARTESIAN_POINT('',(2.5,-3.,2.5));
#8518=CARTESIAN_POINT('Origin',(-2.5,-3.,2.5));
#8519=CARTESIAN_POINT('',(-2.5,-3.,2.5));
#8520=CARTESIAN_POINT('',(-2.5,-3.,2.5));
#8521=CARTESIAN_POINT('',(-2.5,-3.,2.5));
#8522=CARTESIAN_POINT('Origin',(-2.5,-0.025,2.5));
#8523=CARTESIAN_POINT('',(-2.5,-0.025,2.5));
#8524=CARTESIAN_POINT('Origin',(0.,-1.5125,2.5));
#8525=CARTESIAN_POINT('',(0.,0.,0.));
#8526=CARTESIAN_POINT('Origin',(-1.3,1.,6.8));
#8527=CARTESIAN_POINT('',(-1.465,1.,6.8));
#8528=CARTESIAN_POINT('Origin',(-1.3,1.,6.8));
#8529=CARTESIAN_POINT('',(-1.465,1.,7.5));
#8530=CARTESIAN_POINT('',(-1.465,1.,6.8));
#8531=CARTESIAN_POINT('Origin',(-1.3,1.,7.5));
#8532=CARTESIAN_POINT('Origin',(-1.3,1.,6.8));
#8533=CARTESIAN_POINT('Origin',(1.3,1.,6.8));
#8534=CARTESIAN_POINT('',(1.135,1.,6.8));
#8535=CARTESIAN_POINT('Origin',(1.3,1.,6.8));
#8536=CARTESIAN_POINT('',(1.135,1.,7.5));
#8537=CARTESIAN_POINT('',(1.135,1.,6.8));
#8538=CARTESIAN_POINT('Origin',(1.3,1.,7.5));
#8539=CARTESIAN_POINT('Origin',(1.3,1.,6.8));
#8540=CARTESIAN_POINT('Origin',(1.9,-3.1,3.1));
#8541=CARTESIAN_POINT('',(1.625,0.0249999999999999,3.1));
#8542=CARTESIAN_POINT('Origin',(1.9,0.0249999999999999,3.1));
#8543=CARTESIAN_POINT('',(1.625,3.,3.1));
#8544=CARTESIAN_POINT('',(1.625,-3.1,3.1));
#8545=CARTESIAN_POINT('Origin',(1.9,3.,3.1));
#8546=CARTESIAN_POINT('Origin',(-1.9,-3.1,6.9));
#8547=CARTESIAN_POINT('',(-2.175,0.0249999999999999,6.9));
#8548=CARTESIAN_POINT('Origin',(-1.9,0.0249999999999999,6.9));
#8549=CARTESIAN_POINT('',(-2.175,3.,6.9));
#8550=CARTESIAN_POINT('',(-2.175,-3.1,6.9));
#8551=CARTESIAN_POINT('Origin',(-1.9,3.,6.9));
#8552=CARTESIAN_POINT('Origin',(-1.9,-3.1,3.1));
#8553=CARTESIAN_POINT('',(-2.175,0.0249999999999999,3.1));
#8554=CARTESIAN_POINT('Origin',(-1.9,0.0249999999999999,3.1));
#8555=CARTESIAN_POINT('',(-2.175,3.,3.1));
#8556=CARTESIAN_POINT('',(-2.175,-3.1,3.1));
#8557=CARTESIAN_POINT('Origin',(-1.9,3.,3.1));
#8558=CARTESIAN_POINT('Origin',(1.9,-3.1,6.9));
#8559=CARTESIAN_POINT('',(1.625,0.0249999999999999,6.9));
#8560=CARTESIAN_POINT('Origin',(1.9,0.0249999999999999,6.9));
#8561=CARTESIAN_POINT('',(1.625,3.,6.9));
#8562=CARTESIAN_POINT('',(1.625,-3.1,6.9));
#8563=CARTESIAN_POINT('Origin',(1.9,3.,6.9));
#8564=CARTESIAN_POINT('Origin',(0.,0.,6.5));
#8565=CARTESIAN_POINT('',(-0.699553428981661,0.025,6.5));
#8566=CARTESIAN_POINT('',(-0.699553428981661,0.025,7.5));
#8567=CARTESIAN_POINT('',(-0.699553428981661,0.025,6.5));
#8568=CARTESIAN_POINT('',(0.699553428981661,0.025,6.5));
#8569=CARTESIAN_POINT('Origin',(0.,0.,6.5));
#8570=CARTESIAN_POINT('',(0.699553428981661,0.025,7.5));
#8571=CARTESIAN_POINT('',(0.699553428981661,0.025,6.5));
#8572=CARTESIAN_POINT('Origin',(0.,0.,7.5));
#8573=CARTESIAN_POINT('Origin',(0.,0.,6.5));
#8574=CARTESIAN_POINT('',(-0.556214886532175,0.025,6.5));
#8575=CARTESIAN_POINT('',(-1.25,0.025,6.5));
#8576=CARTESIAN_POINT('',(0.556214886532175,0.025,6.5));
#8577=CARTESIAN_POINT('Origin',(0.,0.,6.5));
#8578=CARTESIAN_POINT('',(-1.25,0.025,6.5));
#8579=CARTESIAN_POINT('Origin',(0.,1.5125,7.5));
#8580=CARTESIAN_POINT('',(2.5,0.0249999999999999,7.5));
#8581=CARTESIAN_POINT('',(-2.5,0.025,7.5));
#8582=CARTESIAN_POINT('',(2.5,3.,7.5));
#8583=CARTESIAN_POINT('',(2.5,0.025,7.5));
#8584=CARTESIAN_POINT('',(-2.5,3.,7.5));
#8585=CARTESIAN_POINT('',(2.5,3.,7.5));
#8586=CARTESIAN_POINT('',(-2.5,0.0249999999999999,7.5));
#8587=CARTESIAN_POINT('',(-2.5,3.,7.5));
#8588=CARTESIAN_POINT('',(-2.5,0.025,7.5));
#8589=CARTESIAN_POINT('Origin',(0.,1.8,5.));
#8590=CARTESIAN_POINT('',(-0.93,1.8,5.));
#8591=CARTESIAN_POINT('Origin',(0.,1.8,5.));
#8592=CARTESIAN_POINT('',(-0.93,3.,5.));
#8593=CARTESIAN_POINT('',(-0.93,1.8,5.));
#8594=CARTESIAN_POINT('Origin',(0.,3.,5.));
#8595=CARTESIAN_POINT('Origin',(0.,1.,5.));
#8596=CARTESIAN_POINT('',(-1.3,1.,5.));
#8597=CARTESIAN_POINT('Origin',(0.,1.,5.));
#8598=CARTESIAN_POINT('',(-1.3,1.8,5.));
#8599=CARTESIAN_POINT('',(-1.3,1.,5.));
#8600=CARTESIAN_POINT('Origin',(0.,1.8,5.));
#8601=CARTESIAN_POINT('Origin',(0.,1.8,5.));
#8602=CARTESIAN_POINT('Origin',(0.,1.,5.));
#8603=CARTESIAN_POINT('',(-1.52958336188405E-16,1.,3.75100040032032));
#8604=CARTESIAN_POINT('Origin',(0.,1.,5.));
#8605=CARTESIAN_POINT('Origin',(0.,0.,5.));
#8606=CARTESIAN_POINT('Origin',(0.,0.025,5.));
#8607=CARTESIAN_POINT('Origin',(2.5,3.,2.5));
#8608=CARTESIAN_POINT('',(2.5,3.,2.5));
#8609=CARTESIAN_POINT('',(-2.5,3.,2.5));
#8610=CARTESIAN_POINT('',(2.5,3.,2.5));
#8611=CARTESIAN_POINT('',(-2.5,3.,2.5));
#8612=CARTESIAN_POINT('',(2.5,3.,2.5));
#8613=CARTESIAN_POINT('Origin',(2.5,0.025,2.5));
#8614=CARTESIAN_POINT('',(2.5,0.025,2.5));
#8615=CARTESIAN_POINT('',(2.5,0.025,2.5));
#8616=CARTESIAN_POINT('',(2.5,0.025,2.5));
#8617=CARTESIAN_POINT('Origin',(-2.5,0.025,2.5));
#8618=CARTESIAN_POINT('',(-2.5,0.0249999999999999,2.5));
#8619=CARTESIAN_POINT('',(-2.5,0.0249999999999999,2.5));
#8620=CARTESIAN_POINT('',(-2.5,0.025,2.5));
#8621=CARTESIAN_POINT('Origin',(-2.5,3.,2.5));
#8622=CARTESIAN_POINT('',(-2.5,3.,2.5));
#8623=CARTESIAN_POINT('Origin',(0.,1.5125,2.5));
#8624=CARTESIAN_POINT('',(0.,0.,0.));
#8625=CARTESIAN_POINT('Origin',(1.9,-0.1,3.1));
#8626=CARTESIAN_POINT('',(1.625,-0.025,3.1));
#8627=CARTESIAN_POINT('Origin',(1.9,-0.025,3.1));
#8628=CARTESIAN_POINT('',(1.625,0.025,3.1));
#8629=CARTESIAN_POINT('',(1.625,-0.1,3.1));
#8630=CARTESIAN_POINT('Origin',(1.9,0.025,3.1));
#8631=CARTESIAN_POINT('Origin',(-1.9,-0.1,6.9));
#8632=CARTESIAN_POINT('',(-2.175,-0.025,6.9));
#8633=CARTESIAN_POINT('Origin',(-1.9,-0.025,6.9));
#8634=CARTESIAN_POINT('',(-2.175,0.025,6.9));
#8635=CARTESIAN_POINT('',(-2.175,-0.1,6.9));
#8636=CARTESIAN_POINT('Origin',(-1.9,0.025,6.9));
#8637=CARTESIAN_POINT('Origin',(-1.9,-0.1,3.1));
#8638=CARTESIAN_POINT('',(-2.175,-0.025,3.1));
#8639=CARTESIAN_POINT('Origin',(-1.9,-0.025,3.1));
#8640=CARTESIAN_POINT('',(-2.175,0.025,3.1));
#8641=CARTESIAN_POINT('',(-2.175,-0.1,3.1));
#8642=CARTESIAN_POINT('Origin',(-1.9,0.025,3.1));
#8643=CARTESIAN_POINT('Origin',(1.9,-0.1,6.9));
#8644=CARTESIAN_POINT('',(1.625,-0.025,6.9));
#8645=CARTESIAN_POINT('Origin',(1.9,-0.025,6.9));
#8646=CARTESIAN_POINT('',(1.625,0.025,6.9));
#8647=CARTESIAN_POINT('',(1.625,-0.1,6.9));
#8648=CARTESIAN_POINT('Origin',(1.9,0.025,6.9));
#8649=CARTESIAN_POINT('Origin',(-0.7,-0.1,6.5));
#8650=CARTESIAN_POINT('',(-0.7,-0.025,6.5));
#8651=CARTESIAN_POINT('',(-0.7,-0.025,7.5));
#8652=CARTESIAN_POINT('',(-0.7,-0.025,5.75));
#8653=CARTESIAN_POINT('',(-0.7,0.025,6.5));
#8654=CARTESIAN_POINT('',(-0.7,-0.1,6.5));
#8655=CARTESIAN_POINT('',(-0.7,0.025,7.5));
#8656=CARTESIAN_POINT('',(-0.7,0.025,5.75));
#8657=CARTESIAN_POINT('',(-0.7,-0.0625,7.5));
#8658=CARTESIAN_POINT('Origin',(0.7,-0.1,6.5));
#8659=CARTESIAN_POINT('',(0.7,-0.025,6.5));
#8660=CARTESIAN_POINT('',(0.556776436283003,-0.025,6.5));
#8661=CARTESIAN_POINT('',(0.35,-0.025,6.5));
#8662=CARTESIAN_POINT('',(0.7,0.025,6.5));
#8663=CARTESIAN_POINT('',(0.7,-0.1,6.5));
#8664=CARTESIAN_POINT('',(0.556776436283003,0.025,6.5));
#8665=CARTESIAN_POINT('',(0.35,0.025,6.5));
#8666=CARTESIAN_POINT('',(0.556776436283003,-0.1,6.5));
#8667=CARTESIAN_POINT('Origin',(0.7,-0.1,6.5));
#8668=CARTESIAN_POINT('',(-0.556776436283003,-0.025,6.5));
#8669=CARTESIAN_POINT('',(0.35,-0.025,6.5));
#8670=CARTESIAN_POINT('',(-0.556776436283003,0.025,6.5));
#8671=CARTESIAN_POINT('',(-0.556776436283003,-0.1,6.5));
#8672=CARTESIAN_POINT('',(0.35,0.025,6.5));
#8673=CARTESIAN_POINT('Origin',(0.7,-0.1,7.6));
#8674=CARTESIAN_POINT('',(0.7,-0.025,7.5));
#8675=CARTESIAN_POINT('',(0.7,-0.025,6.3));
#8676=CARTESIAN_POINT('',(0.7,0.025,7.5));
#8677=CARTESIAN_POINT('',(0.7,-0.0625,7.5));
#8678=CARTESIAN_POINT('',(0.7,0.025,6.3));
#8679=CARTESIAN_POINT('Origin',(0.,0.025,5.));
#8680=CARTESIAN_POINT('Origin',(0.,0.025,5.));
#8681=CARTESIAN_POINT('',(2.5,0.025,7.5));
#8682=CARTESIAN_POINT('',(2.5,0.025,7.5));
#8683=CARTESIAN_POINT('',(2.5,0.025,2.5));
#8684=CARTESIAN_POINT('',(2.5,0.025,2.5));
#8685=CARTESIAN_POINT('',(-2.5,0.025,2.5));
#8686=CARTESIAN_POINT('',(-2.5,0.025,2.5));
#8687=CARTESIAN_POINT('',(-2.5,0.025,7.5));
#8688=CARTESIAN_POINT('',(-2.5,0.025,7.5));
#8689=CARTESIAN_POINT('',(2.5,0.025,7.5));
#8690=CARTESIAN_POINT('Origin',(-2.5,-0.025,7.5));
#8691=CARTESIAN_POINT('',(2.5,-0.025,7.5));
#8692=CARTESIAN_POINT('',(2.5,-0.025,7.5));
#8693=CARTESIAN_POINT('',(2.5,-0.025,7.5));
#8694=CARTESIAN_POINT('Origin',(-2.5,-0.025,7.5));
#8695=CARTESIAN_POINT('',(-2.5,-0.025,7.5));
#8696=CARTESIAN_POINT('',(-2.5,-0.025,7.5));
#8697=CARTESIAN_POINT('',(2.5,-0.025,7.5));
#8698=CARTESIAN_POINT('Origin',(0.,-0.1,5.));
#8699=CARTESIAN_POINT('Origin',(0.,-0.025,5.));
#8700=CARTESIAN_POINT('Origin',(-2.5,-0.025,2.5));
#8701=CARTESIAN_POINT('',(-2.5,-0.025,2.5));
#8702=CARTESIAN_POINT('',(-2.5,-0.025,7.5));
#8703=CARTESIAN_POINT('',(-2.5,-0.025,2.5));
#8704=CARTESIAN_POINT('Origin',(2.5,-0.025,2.5));
#8705=CARTESIAN_POINT('',(2.5,-0.025,2.5));
#8706=CARTESIAN_POINT('',(-2.5,-0.025,2.5));
#8707=CARTESIAN_POINT('',(2.5,-0.025,2.5));
#8708=CARTESIAN_POINT('Origin',(2.5,-0.025,7.5));
#8709=CARTESIAN_POINT('',(2.5,-0.025,2.5));
#8710=CARTESIAN_POINT('Origin',(0.,-0.025,5.));
#8711=CARTESIAN_POINT('',(0.,0.,0.));
#8712=CARTESIAN_POINT('Origin',(0.,0.,7.5));
#8713=CARTESIAN_POINT('',(-1.2,-1.46957615897682E-16,7.5));
#8714=CARTESIAN_POINT('Origin',(0.,0.,7.5));
#8715=CARTESIAN_POINT('',(-0.7,-8.57252759403147E-17,7.5));
#8716=CARTESIAN_POINT('Origin',(0.,0.,7.5));
#8717=CARTESIAN_POINT('Origin',(0.,0.,7.5));
#8718=CARTESIAN_POINT('',(-1.2,-1.46957615897682E-16,8.));
#8719=CARTESIAN_POINT('Origin',(0.,0.,8.));
#8720=CARTESIAN_POINT('',(-1.2,-1.46957615897682E-16,7.5));
#8721=CARTESIAN_POINT('Origin',(0.,0.,8.));
#8722=CARTESIAN_POINT('',(-0.405,-4.95981953654678E-17,8.));
#8723=CARTESIAN_POINT('Origin',(0.,0.,8.));
#8724=CARTESIAN_POINT('Origin',(0.,0.,6.6));
#8725=CARTESIAN_POINT('',(-0.405,-4.95981953654678E-17,6.6));
#8726=CARTESIAN_POINT('',(-0.405,-4.95981953654678E-17,6.6));
#8727=CARTESIAN_POINT('Origin',(0.,0.,6.6));
#8728=CARTESIAN_POINT('Origin',(0.,0.,6.6));
#8729=CARTESIAN_POINT('',(-0.7,-8.57252759403147E-17,6.6));
#8730=CARTESIAN_POINT('',(-0.7,-8.57252759403147E-17,6.6));
#8731=CARTESIAN_POINT('Origin',(0.,0.,6.6));
#8732=CARTESIAN_POINT('Origin',(0.,0.,6.6));
#8733=CARTESIAN_POINT('',(0.,0.,0.));
#8734=CARTESIAN_POINT('Origin',(0.,0.,8.1));
#8735=CARTESIAN_POINT('',(-0.4,-4.89858719658941E-17,8.1));
#8736=CARTESIAN_POINT('Origin',(-0.5,-6.12323399573677E-17,8.1));
#8737=CARTESIAN_POINT('Origin',(0.,0.,8.1));
#8738=CARTESIAN_POINT('',(0.,0.,0.));
#8739=CARTESIAN_POINT('Origin',(0.,0.,7.9));
#8740=CARTESIAN_POINT('',(-0.61,-7.47034547479885E-17,8.));
#8741=CARTESIAN_POINT('Origin',(0.,0.,8.));
#8742=CARTESIAN_POINT('',(-0.61,-7.47034547479885E-17,8.3));
#8743=CARTESIAN_POINT('',(-0.61,-7.47034547479885E-17,7.9));
#8744=CARTESIAN_POINT('Origin',(0.,0.,8.3));
#8745=CARTESIAN_POINT('Origin',(0.,0.,8.3));
#8746=CARTESIAN_POINT('',(-0.405,4.95981953654678E-17,8.3));
#8747=CARTESIAN_POINT('Origin',(0.,0.,8.3));
#8748=CARTESIAN_POINT('Origin',(0.,0.,8.));
#8749=CARTESIAN_POINT('',(-0.405,-4.95981953654678E-17,8.7));
#8750=CARTESIAN_POINT('Origin',(0.,0.,8.7));
#8751=CARTESIAN_POINT('',(-0.405,-4.95981953654678E-17,8.));
#8752=CARTESIAN_POINT('Origin',(0.,0.,8.));
#8753=CARTESIAN_POINT('',(-1.,-1.22464679914735E-16,8.7));
#8754=CARTESIAN_POINT('Origin',(0.,0.,8.7));
#8755=CARTESIAN_POINT('',(-1.,-1.22464679914735E-16,8.));
#8756=CARTESIAN_POINT('',(-1.,-1.22464679914735E-16,8.));
#8757=CARTESIAN_POINT('Origin',(0.,0.,8.));
#8758=CARTESIAN_POINT('Origin',(0.,0.,8.7));
#8759=CARTESIAN_POINT('Origin',(0.,0.,8.));
#8760=CARTESIAN_POINT('',(0.,0.,0.));
#8761=CARTESIAN_POINT('Origin',(-1.1,-3.,8.1));
#8762=CARTESIAN_POINT('',(-1.4,-3.,8.1));
#8763=CARTESIAN_POINT('Origin',(-1.1,-3.,8.1));
#8764=CARTESIAN_POINT('',(-1.4,-3.,8.5));
#8765=CARTESIAN_POINT('',(-1.4,-3.,8.1));
#8766=CARTESIAN_POINT('Origin',(-1.1,-3.,8.5));
#8767=CARTESIAN_POINT('Origin',(-1.1,-3.,8.1));
#8768=CARTESIAN_POINT('Origin',(3.,1.1,8.1));
#8769=CARTESIAN_POINT('',(2.7,1.1,8.1));
#8770=CARTESIAN_POINT('Origin',(3.,1.1,8.1));
#8771=CARTESIAN_POINT('',(2.7,1.1,8.5));
#8772=CARTESIAN_POINT('',(2.7,1.1,8.1));
#8773=CARTESIAN_POINT('Origin',(3.,1.1,8.5));
#8774=CARTESIAN_POINT('Origin',(3.,1.1,8.1));
#8775=CARTESIAN_POINT('Origin',(1.3,-1.,7.9));
#8776=CARTESIAN_POINT('',(1.075,-1.,8.));
#8777=CARTESIAN_POINT('Origin',(1.3,-1.,8.));
#8778=CARTESIAN_POINT('',(1.075,-1.,8.5));
#8779=CARTESIAN_POINT('',(1.075,-1.,7.9));
#8780=CARTESIAN_POINT('Origin',(1.3,-1.,8.5));
#8781=CARTESIAN_POINT('Origin',(-1.3,1.,7.9));
#8782=CARTESIAN_POINT('',(-1.525,1.,8.));
#8783=CARTESIAN_POINT('Origin',(-1.3,1.,8.));
#8784=CARTESIAN_POINT('',(-1.525,1.,8.5));
#8785=CARTESIAN_POINT('',(-1.525,1.,7.9));
#8786=CARTESIAN_POINT('Origin',(-1.3,1.,8.5));
#8787=CARTESIAN_POINT('Origin',(-1.3,-1.,7.9));
#8788=CARTESIAN_POINT('',(-1.525,-1.,8.));
#8789=CARTESIAN_POINT('Origin',(-1.3,-1.,8.));
#8790=CARTESIAN_POINT('',(-1.525,-1.,8.5));
#8791=CARTESIAN_POINT('',(-1.525,-1.,7.9));
#8792=CARTESIAN_POINT('Origin',(-1.3,-1.,8.5));
#8793=CARTESIAN_POINT('Origin',(1.3,1.,7.9));
#8794=CARTESIAN_POINT('',(1.075,1.,8.));
#8795=CARTESIAN_POINT('Origin',(1.3,1.,8.));
#8796=CARTESIAN_POINT('',(1.075,1.,8.5));
#8797=CARTESIAN_POINT('',(1.075,1.,7.9));
#8798=CARTESIAN_POINT('Origin',(1.3,1.,8.5));
#8799=CARTESIAN_POINT('Origin',(0.,0.,7.9));
#8800=CARTESIAN_POINT('',(-1.01,-1.23689326713883E-16,8.));
#8801=CARTESIAN_POINT('Origin',(0.,0.,8.));
#8802=CARTESIAN_POINT('',(-1.01,1.23689326713883E-16,8.5));
#8803=CARTESIAN_POINT('',(-1.01,-1.23689326713883E-16,7.9));
#8804=CARTESIAN_POINT('Origin',(0.,0.,8.5));
#8805=CARTESIAN_POINT('Origin',(4.,1.5,8.));
#8806=CARTESIAN_POINT('',(4.,1.5,8.));
#8807=CARTESIAN_POINT('',(-2.5,1.5,8.));
#8808=CARTESIAN_POINT('',(4.,1.5,8.));
#8809=CARTESIAN_POINT('',(-2.5,1.5,8.5));
#8810=CARTESIAN_POINT('',(-2.5,1.5,8.));
#8811=CARTESIAN_POINT('',(4.,1.5,8.5));
#8812=CARTESIAN_POINT('',(4.,1.5,8.5));
#8813=CARTESIAN_POINT('',(4.,1.5,8.));
#8814=CARTESIAN_POINT('Origin',(4.,-4.,8.));
#8815=CARTESIAN_POINT('',(4.,-4.,8.));
#8816=CARTESIAN_POINT('',(4.,-4.,8.));
#8817=CARTESIAN_POINT('',(4.,-4.,8.5));
#8818=CARTESIAN_POINT('',(4.,-4.,8.5));
#8819=CARTESIAN_POINT('',(4.,-4.,8.));
#8820=CARTESIAN_POINT('Origin',(-2.5,-4.,8.));
#8821=CARTESIAN_POINT('',(-2.5,-4.,8.));
#8822=CARTESIAN_POINT('',(-2.5,-4.,8.));
#8823=CARTESIAN_POINT('',(-2.5,-4.,8.5));
#8824=CARTESIAN_POINT('',(-2.5,-4.,8.5));
#8825=CARTESIAN_POINT('',(-2.5,-4.,8.));
#8826=CARTESIAN_POINT('Origin',(-2.5,1.5,8.));
#8827=CARTESIAN_POINT('',(-2.5,1.5,8.));
#8828=CARTESIAN_POINT('',(-2.5,1.5,8.5));
#8829=CARTESIAN_POINT('Origin',(0.75,-1.25,8.5));
#8830=CARTESIAN_POINT('Origin',(0.75,-1.25,8.));
#8831=CARTESIAN_POINT('',(0.,0.,0.));
#8832=CARTESIAN_POINT('Origin',(0.,0.,5.));
#8833=CARTESIAN_POINT('',(-1.36919674566051E-16,-1.,6.11803398874989));
#8834=CARTESIAN_POINT('Origin',(0.,-1.,5.));
#8835=CARTESIAN_POINT('',(-0.75,-1.29903810567666,5.));
#8836=CARTESIAN_POINT('Origin',(0.,-1.29903810567666,5.));
#8837=CARTESIAN_POINT('Origin',(0.,-1.8,5.));
#8838=CARTESIAN_POINT('',(-0.75,-1.8,5.));
#8839=CARTESIAN_POINT('',(-0.75,-1.8,5.));
#8840=CARTESIAN_POINT('Origin',(0.,-1.8,5.));
#8841=CARTESIAN_POINT('Origin',(0.,-1.8,5.));
#8842=CARTESIAN_POINT('',(-1.3,-1.,5.));
#8843=CARTESIAN_POINT('Origin',(0.,-1.,5.));
#8844=CARTESIAN_POINT('',(-1.3,-1.8,5.));
#8845=CARTESIAN_POINT('',(-1.3,-1.8,5.));
#8846=CARTESIAN_POINT('Origin',(0.,-1.8,5.));
#8847=CARTESIAN_POINT('Origin',(0.,-1.,5.));
#8848=CARTESIAN_POINT('Origin',(0.,-1.8,5.));
#8849=CARTESIAN_POINT('',(0.,0.,0.));
#8850=CARTESIAN_POINT('Origin',(0.115470053837925,-0.5,-0.2));
#8851=CARTESIAN_POINT('',(0.23094010767585,-0.5,0.));
#8852=CARTESIAN_POINT('',(0.115470053837925,-0.5,-0.2));
#8853=CARTESIAN_POINT('',(0.23094010767585,-0.5,0.));
#8854=CARTESIAN_POINT('',(0.115470053837925,-0.8,-0.2));
#8855=CARTESIAN_POINT('',(0.115470053837925,-0.5,-0.2));
#8856=CARTESIAN_POINT('',(0.23094010767585,-0.8,0.));
#8857=CARTESIAN_POINT('',(0.23094010767585,-0.8,0.));
#8858=CARTESIAN_POINT('',(0.23094010767585,-0.5,0.));
#8859=CARTESIAN_POINT('Origin',(-0.115470053837925,-0.5,-0.2));
#8860=CARTESIAN_POINT('',(-0.115470053837925,-0.5,-0.2));
#8861=CARTESIAN_POINT('',(0.115470053837925,-0.5,-0.2));
#8862=CARTESIAN_POINT('',(-0.115470053837925,-0.8,-0.2));
#8863=CARTESIAN_POINT('',(-0.115470053837925,-0.5,-0.2));
#8864=CARTESIAN_POINT('',(0.115470053837925,-0.8,-0.2));
#8865=CARTESIAN_POINT('Origin',(-0.23094010767585,-0.5,-2.77555756156289E-17));
#8866=CARTESIAN_POINT('',(-0.23094010767585,-0.5,-2.82820063659975E-17));
#8867=CARTESIAN_POINT('',(-0.115470053837925,-0.5,-0.2));
#8868=CARTESIAN_POINT('',(-0.23094010767585,-0.8,-2.77555756156289E-17));
#8869=CARTESIAN_POINT('',(-0.23094010767585,-0.5,-2.82820063659975E-17));
#8870=CARTESIAN_POINT('',(-0.115470053837925,-0.8,-0.2));
#8871=CARTESIAN_POINT('Origin',(-0.115470053837925,-0.5,0.2));
#8872=CARTESIAN_POINT('',(-0.115470053837925,-0.5,0.2));
#8873=CARTESIAN_POINT('',(-0.23094010767585,-0.5,-2.82820063659975E-17));
#8874=CARTESIAN_POINT('',(-0.115470053837925,-0.8,0.2));
#8875=CARTESIAN_POINT('',(-0.115470053837925,-0.5,0.2));
#8876=CARTESIAN_POINT('',(-0.23094010767585,-0.8,-2.82820063659975E-17));
#8877=CARTESIAN_POINT('Origin',(0.115470053837925,-0.5,0.2));
#8878=CARTESIAN_POINT('',(0.115470053837925,-0.5,0.2));
#8879=CARTESIAN_POINT('',(-0.115470053837925,-0.5,0.2));
#8880=CARTESIAN_POINT('',(0.115470053837925,-0.8,0.2));
#8881=CARTESIAN_POINT('',(0.115470053837925,-0.5,0.2));
#8882=CARTESIAN_POINT('',(-0.115470053837925,-0.8,0.2));
#8883=CARTESIAN_POINT('Origin',(0.23094010767585,-0.5,0.));
#8884=CARTESIAN_POINT('',(0.115470053837925,-0.5,0.2));
#8885=CARTESIAN_POINT('',(0.115470053837925,-0.8,0.2));
#8886=CARTESIAN_POINT('Origin',(0.,-0.5,0.));
#8887=CARTESIAN_POINT('Origin',(0.,-0.8,0.));
#8888=CARTESIAN_POINT('Origin',(0.,-1.9,0.));
#8889=CARTESIAN_POINT('',(-0.25,-1.9,3.06161699786838E-17));
#8890=CARTESIAN_POINT('Origin',(0.,-1.9,0.));
#8891=CARTESIAN_POINT('',(-0.24505,-1.9,3.00099698131059E-17));
#8892=CARTESIAN_POINT('Origin',(0.,-1.9,0.));
#8893=CARTESIAN_POINT('Origin',(0.,-7.,0.));
#8894=CARTESIAN_POINT('',(-0.25,-7.,3.06161699786838E-17));
#8895=CARTESIAN_POINT('',(-0.25,-7.,3.06161699786838E-17));
#8896=CARTESIAN_POINT('Origin',(0.,-7.,0.));
#8897=CARTESIAN_POINT('Origin',(0.,-7.,0.));
#8898=CARTESIAN_POINT('Origin',(0.375,0.5,0.));
#8899=CARTESIAN_POINT('',(-0.375,0.5,-4.59242549680257E-17));
#8900=CARTESIAN_POINT('Origin',(0.,0.5,0.));
#8901=CARTESIAN_POINT('Origin',(0.,0.475,0.));
#8902=CARTESIAN_POINT('',(-0.425,0.45,-5.20474889637625E-17));
#8903=CARTESIAN_POINT('Origin',(0.,0.45,0.));
#8904=CARTESIAN_POINT('',(-0.4,0.475,-4.89858719658941E-17));
#8905=CARTESIAN_POINT('Origin',(0.,0.24,0.));
#8906=CARTESIAN_POINT('',(-0.425,0.0299999999999998,-5.20474889637625E-17));
#8907=CARTESIAN_POINT('Origin',(0.,0.0299999999999998,0.));
#8908=CARTESIAN_POINT('',(-0.425,0.24,-5.20474889637625E-17));
#8909=CARTESIAN_POINT('Origin',(0.,0.0150000000000001,0.));
#8910=CARTESIAN_POINT('',(-0.395,4.85722573273506E-17,-4.83735485663204E-17));
#8911=CARTESIAN_POINT('Origin',(0.,0.,0.));
#8912=CARTESIAN_POINT('',(-0.41,0.0150000000000001,-5.02105187650415E-17));
#8913=CARTESIAN_POINT('Origin',(0.27,0.,0.));
#8914=CARTESIAN_POINT('',(-0.27,0.,-3.30654635769785E-17));
#8915=CARTESIAN_POINT('Origin',(0.,0.,0.));
#8916=CARTESIAN_POINT('Origin',(0.,-0.02,0.));
#8917=CARTESIAN_POINT('',(-0.24505,-0.0498999999999999,3.00099698131059E-17));
#8918=CARTESIAN_POINT('Origin',(0.,-0.0498999999999999,0.));
#8919=CARTESIAN_POINT('',(-0.26,-0.02,-3.18408167778312E-17));
#8920=CARTESIAN_POINT('Origin',(0.,-0.995,0.));
#8921=CARTESIAN_POINT('',(-0.24505,-0.995,-3.00099698131059E-17));
#8922=CARTESIAN_POINT('',(0.,0.,0.));
#8923=CARTESIAN_POINT('Origin',(0.,0.09,0.));
#8924=CARTESIAN_POINT('',(-0.285,0.1,3.49024337756996E-17));
#8925=CARTESIAN_POINT('Origin',(0.,0.1,0.));
#8926=CARTESIAN_POINT('',(-0.265,0.08,-3.24531401774049E-17));
#8927=CARTESIAN_POINT('',(-0.275,0.09,3.36777869765522E-17));
#8928=CARTESIAN_POINT('Origin',(0.,0.08,0.));
#8929=CARTESIAN_POINT('Origin',(0.,0.,0.));
#8930=CARTESIAN_POINT('',(-0.265,0.,3.24531401774049E-17));
#8931=CARTESIAN_POINT('',(-0.265,0.,3.24531401774049E-17));
#8932=CARTESIAN_POINT('Origin',(0.,0.,0.));
#8933=CARTESIAN_POINT('Origin',(0.,0.1,0.));
#8934=CARTESIAN_POINT('',(-0.5,0.1,6.12323399573677E-17));
#8935=CARTESIAN_POINT('Origin',(0.,0.1,0.));
#8936=CARTESIAN_POINT('Origin',(0.,0.,0.));
#8937=CARTESIAN_POINT('',(-0.5,0.,6.12323399573677E-17));
#8938=CARTESIAN_POINT('',(-0.5,0.,6.12323399573677E-17));
#8939=CARTESIAN_POINT('Origin',(0.,0.,0.));
#8940=CARTESIAN_POINT('Origin',(0.,0.,0.));
#8941=CARTESIAN_POINT('',(0.,0.,0.));
#8942=CARTESIAN_POINT('Origin',(0.,0.0525042956467857,0.));
#8943=CARTESIAN_POINT('',(-0.230940107675851,0.0472735643746089,0.4));
#8944=CARTESIAN_POINT('',(0.23094010767585,0.0472735643746089,0.4));
#8945=CARTESIAN_POINT('Ctrl Pts',(-0.230940107675851,0.0472735643746089,
0.4));
#8946=CARTESIAN_POINT('Ctrl Pts',(1.11022302462516E-16,-0.0193931022920578,
0.4));
#8947=CARTESIAN_POINT('Ctrl Pts',(0.23094010767585,0.0472735643746089,0.4));
#8948=CARTESIAN_POINT('',(-0.461880215351701,0.0472735643746089,-5.6564012731995E-17));
#8949=CARTESIAN_POINT('Ctrl Pts',(-0.461880215351701,0.0472735643746089,
-5.6564012731995E-17));
#8950=CARTESIAN_POINT('Ctrl Pts',(-0.346410161513776,-0.0193931022920579,
0.2));
#8951=CARTESIAN_POINT('Ctrl Pts',(-0.230940107675851,0.0472735643746089,
0.4));
#8952=CARTESIAN_POINT('',(-0.38,-2.08166817117217E-17,-4.65365783675994E-17));
#8953=CARTESIAN_POINT('',(-0.47094010767585,0.0525042956467857,-5.7673529545534E-17));
#8954=CARTESIAN_POINT('Origin',(0.,0.,0.));
#8955=CARTESIAN_POINT('',(-0.23094010767585,0.0472735643746089,-0.4));
#8956=CARTESIAN_POINT('Ctrl Pts',(-0.23094010767585,0.0472735643746089,
-0.4));
#8957=CARTESIAN_POINT('Ctrl Pts',(-0.346410161513775,-0.0193931022920578,
-0.2));
#8958=CARTESIAN_POINT('Ctrl Pts',(-0.461880215351701,0.0472735643746089,
-5.6564012731995E-17));
#8959=CARTESIAN_POINT('',(0.23094010767585,0.0472735643746089,-0.4));
#8960=CARTESIAN_POINT('Ctrl Pts',(0.23094010767585,0.0472735643746089,-0.4));
#8961=CARTESIAN_POINT('Ctrl Pts',(0.,-0.0193931022920578,-0.4));
#8962=CARTESIAN_POINT('Ctrl Pts',(-0.23094010767585,0.0472735643746089,
-0.4));
#8963=CARTESIAN_POINT('',(0.461880215351701,0.0472735643746089,0.));
#8964=CARTESIAN_POINT('Ctrl Pts',(0.461880215351701,0.0472735643746089,
0.));
#8965=CARTESIAN_POINT('Ctrl Pts',(0.346410161513776,-0.019393102292058,
-0.2));
#8966=CARTESIAN_POINT('Ctrl Pts',(0.23094010767585,0.0472735643746089,-0.4));
#8967=CARTESIAN_POINT('Ctrl Pts',(0.23094010767585,0.0472735643746089,0.4));
#8968=CARTESIAN_POINT('Ctrl Pts',(0.346410161513776,-0.0193931022920577,
0.2));
#8969=CARTESIAN_POINT('Ctrl Pts',(0.461880215351701,0.0472735643746089,
0.));
#8970=CARTESIAN_POINT('Origin',(0.,0.417495704353214,0.));
#8971=CARTESIAN_POINT('',(-0.38,0.47,-4.65365783675994E-17));
#8972=CARTESIAN_POINT('Origin',(0.,0.47,0.));
#8973=CARTESIAN_POINT('',(-0.461880215351701,0.422726435625391,-5.6564012731995E-17));
#8974=CARTESIAN_POINT('',(-0.47094010767585,0.417495704353214,-5.7673529545534E-17));
#8975=CARTESIAN_POINT('',(-0.230940107675851,0.422726435625391,0.4));
#8976=CARTESIAN_POINT('Ctrl Pts',(-0.230940107675851,0.422726435625391,
0.4));
#8977=CARTESIAN_POINT('Ctrl Pts',(-0.346410161513776,0.489393102292058,
0.2));
#8978=CARTESIAN_POINT('Ctrl Pts',(-0.461880215351701,0.422726435625391,
-5.6564012731995E-17));
#8979=CARTESIAN_POINT('',(0.23094010767585,0.422726435625391,0.4));
#8980=CARTESIAN_POINT('Ctrl Pts',(0.23094010767585,0.422726435625391,0.4));
#8981=CARTESIAN_POINT('Ctrl Pts',(8.32667268468867E-17,0.489393102292058,
0.4));
#8982=CARTESIAN_POINT('Ctrl Pts',(-0.230940107675851,0.422726435625391,
0.4));
#8983=CARTESIAN_POINT('',(0.461880215351701,0.422726435625391,0.));
#8984=CARTESIAN_POINT('Ctrl Pts',(0.461880215351701,0.422726435625391,0.));
#8985=CARTESIAN_POINT('Ctrl Pts',(0.346410161513776,0.489393102292058,0.2));
#8986=CARTESIAN_POINT('Ctrl Pts',(0.23094010767585,0.422726435625391,0.4));
#8987=CARTESIAN_POINT('',(0.23094010767585,0.422726435625391,-0.4));
#8988=CARTESIAN_POINT('Ctrl Pts',(0.23094010767585,0.422726435625391,-0.4));
#8989=CARTESIAN_POINT('Ctrl Pts',(0.346410161513775,0.489393102292058,-0.2));
#8990=CARTESIAN_POINT('Ctrl Pts',(0.461880215351701,0.422726435625391,0.));
#8991=CARTESIAN_POINT('',(-0.23094010767585,0.422726435625391,-0.4));
#8992=CARTESIAN_POINT('Ctrl Pts',(-0.23094010767585,0.422726435625391,-0.4));
#8993=CARTESIAN_POINT('Ctrl Pts',(-5.55111512312578E-17,0.489393102292058,
-0.4));
#8994=CARTESIAN_POINT('Ctrl Pts',(0.23094010767585,0.422726435625391,-0.4));
#8995=CARTESIAN_POINT('Ctrl Pts',(-0.461880215351701,0.422726435625391,
-5.6564012731995E-17));
#8996=CARTESIAN_POINT('Ctrl Pts',(-0.346410161513776,0.489393102292058,
-0.2));
#8997=CARTESIAN_POINT('Ctrl Pts',(-0.23094010767585,0.422726435625391,-0.4));
#8998=CARTESIAN_POINT('Origin',(0.23094010767585,0.,-0.4));
#8999=CARTESIAN_POINT('',(-0.23094010767585,0.,-0.4));
#9000=CARTESIAN_POINT('',(0.23094010767585,0.,-0.4));
#9001=CARTESIAN_POINT('Origin',(-0.23094010767585,0.,-0.4));
#9002=CARTESIAN_POINT('',(-0.461880215351701,0.,-5.6564012731995E-17));
#9003=CARTESIAN_POINT('Origin',(-0.461880215351701,0.,-5.6564012731995E-17));
#9004=CARTESIAN_POINT('',(-0.230940107675851,0.,0.4));
#9005=CARTESIAN_POINT('Origin',(0.,0.,0.));
#9006=CARTESIAN_POINT('',(-0.2117,0.47,2.59257727379495E-17));
#9007=CARTESIAN_POINT('Origin',(0.,0.47,0.));
#9008=CARTESIAN_POINT('',(-0.2117,0.,2.59257727379495E-17));
#9009=CARTESIAN_POINT('',(-0.2117,0.,2.59257727379495E-17));
#9010=CARTESIAN_POINT('Origin',(0.,0.,0.));
#9011=CARTESIAN_POINT('Origin',(-0.230940107675851,0.,0.4));
#9012=CARTESIAN_POINT('',(0.23094010767585,0.,0.4));
#9013=CARTESIAN_POINT('Origin',(0.461880215351701,0.,0.));
#9014=CARTESIAN_POINT('',(0.461880215351701,0.,0.));
#9015=CARTESIAN_POINT('Origin',(0.23094010767585,0.,0.4));
#9016=CARTESIAN_POINT('Origin',(0.,0.47,0.));
#9017=CARTESIAN_POINT('Origin',(0.,0.,0.));
#9018=CARTESIAN_POINT('',(0.,0.,0.));
#9019=CARTESIAN_POINT('Origin',(-1.3,-1.,7.5));
#9020=CARTESIAN_POINT('',(-1.525,-1.,8.));
#9021=CARTESIAN_POINT('Origin',(-1.3,-1.,8.));
#9022=CARTESIAN_POINT('',(-1.525,-1.,7.5));
#9023=CARTESIAN_POINT('',(-1.525,-1.,7.5));
#9024=CARTESIAN_POINT('Origin',(-1.3,-1.,7.5));
#9025=CARTESIAN_POINT('Origin',(-1.3,-1.,7.5));
#9026=CARTESIAN_POINT('',(-1.7,-1.,8.));
#9027=CARTESIAN_POINT('Origin',(-1.3,-1.,8.));
#9028=CARTESIAN_POINT('',(-1.7,-1.,7.5));
#9029=CARTESIAN_POINT('',(-1.7,-1.,7.5));
#9030=CARTESIAN_POINT('Origin',(-1.3,-1.,7.5));
#9031=CARTESIAN_POINT('Origin',(-1.3,-1.,8.));
#9032=CARTESIAN_POINT('Origin',(-1.3,-1.,7.5));
#9033=CARTESIAN_POINT('',(0.,0.,0.));
#9034=CARTESIAN_POINT('Origin',(0.3,0.4,0.));
#9035=CARTESIAN_POINT('',(-0.3,0.4,-3.67394039744206E-17));
#9036=CARTESIAN_POINT('Origin',(0.,0.4,0.));
#9037=CARTESIAN_POINT('Origin',(0.,0.375,0.));
#9038=CARTESIAN_POINT('',(-0.35,0.35,-4.28626379701573E-17));
#9039=CARTESIAN_POINT('Origin',(0.,0.35,0.));
#9040=CARTESIAN_POINT('',(-0.325,0.375,-3.9801020972289E-17));
#9041=CARTESIAN_POINT('Origin',(0.,0.19,0.));
#9042=CARTESIAN_POINT('',(-0.35,0.03,-4.28626379701574E-17));
#9043=CARTESIAN_POINT('Origin',(0.,0.03,0.));
#9044=CARTESIAN_POINT('',(-0.35,0.19,-4.28626379701574E-17));
#9045=CARTESIAN_POINT('Origin',(0.,0.0149999999999999,0.));
#9046=CARTESIAN_POINT('',(-0.32,-3.29597460435593E-17,-3.91886975727153E-17));
#9047=CARTESIAN_POINT('Origin',(0.,0.,0.));
#9048=CARTESIAN_POINT('',(-0.335,0.0149999999999999,-4.10256677714363E-17));
#9049=CARTESIAN_POINT('Origin',(0.22,0.,0.));
#9050=CARTESIAN_POINT('',(-0.22,-6.93889390390723E-18,-2.69422295812418E-17));
#9051=CARTESIAN_POINT('Origin',(0.,0.,0.));
#9052=CARTESIAN_POINT('Origin',(0.,-0.02,0.));
#9053=CARTESIAN_POINT('',(-0.1954,-0.0492,2.39295984553393E-17));
#9054=CARTESIAN_POINT('Origin',(0.,-0.0492,0.));
#9055=CARTESIAN_POINT('',(-0.21,-0.02,-2.57175827820944E-17));
#9056=CARTESIAN_POINT('Origin',(0.,-0.8,0.));
#9057=CARTESIAN_POINT('',(-0.1954,-1.5646,2.39295984553393E-17));
#9058=CARTESIAN_POINT('Origin',(0.,-1.5646,0.));
#9059=CARTESIAN_POINT('',(-0.1954,-0.8,-2.39295984553393E-17));
#9060=CARTESIAN_POINT('Origin',(0.,-1.58,0.));
#9061=CARTESIAN_POINT('',(-0.16,-1.6,-1.95943487863577E-17));
#9062=CARTESIAN_POINT('Origin',(0.,-1.6,0.));
#9063=CARTESIAN_POINT('',(-0.18,-1.58,-2.20436423846524E-17));
#9064=CARTESIAN_POINT('Origin',(0.,-1.6,0.));
#9065=CARTESIAN_POINT('Origin',(0.0866025403784439,-0.4,-0.15));
#9066=CARTESIAN_POINT('',(0.173205080756888,-0.4,0.));
#9067=CARTESIAN_POINT('',(0.0866025403784439,-0.4,-0.15));
#9068=CARTESIAN_POINT('',(0.173205080756888,-0.4,0.));
#9069=CARTESIAN_POINT('',(0.0866025403784439,-0.64,-0.15));
#9070=CARTESIAN_POINT('',(0.0866025403784439,-0.4,-0.15));
#9071=CARTESIAN_POINT('',(0.173205080756888,-0.64,0.));
#9072=CARTESIAN_POINT('',(0.173205080756888,-0.64,0.));
#9073=CARTESIAN_POINT('',(0.173205080756888,-0.4,0.));
#9074=CARTESIAN_POINT('Origin',(-0.0866025403784438,-0.4,-0.15));
#9075=CARTESIAN_POINT('',(-0.0866025403784438,-0.4,-0.15));
#9076=CARTESIAN_POINT('',(0.0866025403784439,-0.4,-0.15));
#9077=CARTESIAN_POINT('',(-0.0866025403784438,-0.64,-0.15));
#9078=CARTESIAN_POINT('',(-0.0866025403784438,-0.4,-0.15));
#9079=CARTESIAN_POINT('',(0.0866025403784439,-0.64,-0.15));
#9080=CARTESIAN_POINT('Origin',(-0.173205080756888,-0.4,-2.77555756156289E-17));
#9081=CARTESIAN_POINT('',(-0.173205080756888,-0.4,-2.12115047744981E-17));
#9082=CARTESIAN_POINT('',(-0.0866025403784438,-0.4,-0.15));
#9083=CARTESIAN_POINT('',(-0.173205080756888,-0.64,-2.77555756156289E-17));
#9084=CARTESIAN_POINT('',(-0.173205080756888,-0.4,-2.12115047744981E-17));
#9085=CARTESIAN_POINT('',(-0.0866025403784438,-0.64,-0.15));
#9086=CARTESIAN_POINT('Origin',(-0.0866025403784439,-0.4,0.15));
#9087=CARTESIAN_POINT('',(-0.0866025403784439,-0.4,0.15));
#9088=CARTESIAN_POINT('',(-0.173205080756888,-0.4,-2.12115047744981E-17));
#9089=CARTESIAN_POINT('',(-0.0866025403784439,-0.64,0.15));
#9090=CARTESIAN_POINT('',(-0.0866025403784439,-0.4,0.15));
#9091=CARTESIAN_POINT('',(-0.173205080756888,-0.64,-2.12115047744981E-17));
#9092=CARTESIAN_POINT('Origin',(0.0866025403784439,-0.4,0.15));
#9093=CARTESIAN_POINT('',(0.0866025403784439,-0.4,0.15));
#9094=CARTESIAN_POINT('',(-0.0866025403784439,-0.4,0.15));
#9095=CARTESIAN_POINT('',(0.0866025403784439,-0.64,0.15));
#9096=CARTESIAN_POINT('',(0.0866025403784439,-0.4,0.15));
#9097=CARTESIAN_POINT('',(-0.0866025403784439,-0.64,0.15));
#9098=CARTESIAN_POINT('Origin',(0.173205080756888,-0.4,0.));
#9099=CARTESIAN_POINT('',(0.0866025403784439,-0.4,0.15));
#9100=CARTESIAN_POINT('',(0.0866025403784439,-0.64,0.15));
#9101=CARTESIAN_POINT('Origin',(0.,-0.4,-2.77555756156289E-17));
#9102=CARTESIAN_POINT('Origin',(0.,-0.64,-2.77555756156289E-17));
#9103=CARTESIAN_POINT('',(0.,0.,0.));
#9104=CARTESIAN_POINT('Origin',(3.,1.1,8.2));
#9105=CARTESIAN_POINT('',(2.7,1.1,9.4));
#9106=CARTESIAN_POINT('Origin',(3.,1.1,9.4));
#9107=CARTESIAN_POINT('',(2.7,1.1,8.2));
#9108=CARTESIAN_POINT('',(2.7,1.1,8.2));
#9109=CARTESIAN_POINT('Origin',(3.,1.1,8.2));
#9110=CARTESIAN_POINT('Origin',(3.,1.1,9.4));
#9111=CARTESIAN_POINT('Origin',(3.,1.1,8.2));
#9112=CARTESIAN_POINT('',(0.,0.,0.));
#9113=CARTESIAN_POINT('',(0.,0.,0.));
#9114=CARTESIAN_POINT('',(0.,0.,0.));
#9115=CARTESIAN_POINT('',(0.,0.,0.));
#9116=CARTESIAN_POINT('',(0.,0.,0.));
#9117=CARTESIAN_POINT('',(0.,0.,0.));
#9118=CARTESIAN_POINT('',(0.,0.,0.));
#9119=CARTESIAN_POINT('',(0.,0.,0.));
#9120=CARTESIAN_POINT('',(0.,0.,0.));
#9121=CARTESIAN_POINT('',(-1.9,-3.,3.1));
#9122=CARTESIAN_POINT('',(-1.9,-3.1,3.1));
#9123=CARTESIAN_POINT('',(-1.9,3.,3.1));
#9124=CARTESIAN_POINT('',(-1.9,3.1,3.1));
#9125=CARTESIAN_POINT('',(-1.9,-3.,6.9));
#9126=CARTESIAN_POINT('',(-1.9,-3.1,6.9));
#9127=CARTESIAN_POINT('',(-1.9,3.,6.9));
#9128=CARTESIAN_POINT('',(-1.9,3.1,6.9));
#9129=CARTESIAN_POINT('',(1.9,-3.,3.1));
#9130=CARTESIAN_POINT('',(1.9,-3.1,3.1));
#9131=CARTESIAN_POINT('',(1.9,3.,3.1));
#9132=CARTESIAN_POINT('',(1.9,3.1,3.1));
#9133=CARTESIAN_POINT('',(1.9,-3.,6.9));
#9134=CARTESIAN_POINT('',(1.9,-3.1,6.9));
#9135=CARTESIAN_POINT('',(1.9,3.,6.9));
#9136=CARTESIAN_POINT('',(1.9,3.1,6.9));
#9137=CARTESIAN_POINT('',(0.,0.,0.));
#9138=CARTESIAN_POINT('',(-1.3,-1.,8.5));
#9139=CARTESIAN_POINT('',(0.,2.,0.));
#9140=CARTESIAN_POINT('',(-1.3,1.,8.5));
#9141=CARTESIAN_POINT('',(2.6,0.,0.));
#9142=CARTESIAN_POINT('',(1.3,-1.,8.5));
#9143=CARTESIAN_POINT('',(2.6,2.,0.));
#9144=CARTESIAN_POINT('',(1.3,1.,8.5));
#9145=CARTESIAN_POINT('',(0.,0.,0.));
#9146=CARTESIAN_POINT('',(-4.1,-4.1,0.));
#9147=CARTESIAN_POINT('',(0.,0.,0.));
#9148=CARTESIAN_POINT('Origin',(-0.1,0.,6.));
#9149=CARTESIAN_POINT('',(0.1,-9.67470971326409E-17,6.79));
#9150=CARTESIAN_POINT('Origin',(0.1,0.,6.));
#9151=CARTESIAN_POINT('',(-0.1,-9.67470971326409E-17,6.79));
#9152=CARTESIAN_POINT('',(-0.1,-9.67470971326409E-17,6.79));
#9153=CARTESIAN_POINT('Origin',(-0.1,0.,6.));
#9154=CARTESIAN_POINT('Origin',(-0.1,0.,6.));
#9155=CARTESIAN_POINT('',(0.1,-2.69422295812418E-16,8.2));
#9156=CARTESIAN_POINT('Origin',(0.1,0.,6.));
#9157=CARTESIAN_POINT('',(-0.1,-2.69422295812418E-16,8.2));
#9158=CARTESIAN_POINT('',(-0.1,-2.69422295812418E-16,8.2));
#9159=CARTESIAN_POINT('Origin',(-0.1,0.,6.));
#9160=CARTESIAN_POINT('Origin',(0.1,0.,6.));
#9161=CARTESIAN_POINT('Origin',(-0.1,0.,6.));
#9162=CARTESIAN_POINT('',(0.,0.,0.));
#9163=CARTESIAN_POINT('Origin',(-12.,-0.7,5.));
#9164=CARTESIAN_POINT('',(-11.3,-0.7,5.61229078059367));
#9165=CARTESIAN_POINT('',(-11.3,-0.700000000000001,5.36619666847201));
#9166=CARTESIAN_POINT('',(-11.3,-0.7,5.));
#9167=CARTESIAN_POINT('',(-12.7,-0.7,5.61229078059366));
#9168=CARTESIAN_POINT('Origin',(-12.,-0.7,5.));
#9169=CARTESIAN_POINT('',(-12.7,-0.700000000000002,5.36619666847201));
#9170=CARTESIAN_POINT('',(-12.7,-0.7,5.));
#9171=CARTESIAN_POINT('Origin',(-12.,-0.7,5.));
#9172=CARTESIAN_POINT('Origin',(-12.,-2.1,5.));
#9173=CARTESIAN_POINT('',(-12.93,-2.,5.));
#9174=CARTESIAN_POINT('Origin',(-12.,-2.,5.));
#9175=CARTESIAN_POINT('',(-12.93,-0.93,5.));
#9176=CARTESIAN_POINT('',(-12.93,-2.1,5.));
#9177=CARTESIAN_POINT('Origin',(-12.,0.,5.));
#9178=CARTESIAN_POINT('',(-11.3,-0.7,4.38770921940633));
#9179=CARTESIAN_POINT('Origin',(-12.,0.,5.));
#9180=CARTESIAN_POINT('',(-12.7,-0.7,4.38770921940634));
#9181=CARTESIAN_POINT('Origin',(-12.,-0.7,5.));
#9182=CARTESIAN_POINT('Origin',(-12.,0.,5.));
#9183=CARTESIAN_POINT('Origin',(-12.,-0.7,5.));
#9184=CARTESIAN_POINT('',(-11.3,-0.700000000000001,4.63380333152799));
#9185=CARTESIAN_POINT('',(-11.3,-0.7,5.));
#9186=CARTESIAN_POINT('',(-12.7,-0.700000000000002,4.63380333152799));
#9187=CARTESIAN_POINT('Origin',(-12.,-0.7,5.));
#9188=CARTESIAN_POINT('',(-12.7,-0.7,5.));
#9189=CARTESIAN_POINT('Origin',(-11.3,0.,5.));
#9190=CARTESIAN_POINT('',(-11.3,-1.13892152320704E-16,5.93));
#9191=CARTESIAN_POINT('Origin',(-11.3,0.,5.));
#9192=CARTESIAN_POINT('',(-10.,1.13892152320704E-16,5.93));
#9193=CARTESIAN_POINT('',(-11.3,-1.13892152320704E-16,5.93));
#9194=CARTESIAN_POINT('Origin',(-10.,0.,5.));
#9195=CARTESIAN_POINT('Origin',(-11.3,0.,5.));
#9196=CARTESIAN_POINT('Origin',(-12.,-2.1,5.));
#9197=CARTESIAN_POINT('',(-12.,0.,5.79));
#9198=CARTESIAN_POINT('Origin',(-12.,0.,5.));
#9199=CARTESIAN_POINT('Origin',(-12.,0.,5.));
#9200=CARTESIAN_POINT('Origin',(-11.3,0.,5.));
#9201=CARTESIAN_POINT('Origin',(-11.3,0.,5.));
#9202=CARTESIAN_POINT('Origin',(-12.,-2.1,5.));
#9203=CARTESIAN_POINT('',(-12.,0.,4.21));
#9204=CARTESIAN_POINT('Origin',(-12.,0.,5.));
#9205=CARTESIAN_POINT('Origin',(-12.,0.,5.));
#9206=CARTESIAN_POINT('Origin',(-12.7,0.,5.));
#9207=CARTESIAN_POINT('Origin',(-12.7,0.,5.));
#9208=CARTESIAN_POINT('',(-12.7,-1.13892152320704E-16,5.93));
#9209=CARTESIAN_POINT('Origin',(-12.7,0.,5.));
#9210=CARTESIAN_POINT('Origin',(-12.7,0.,5.));
#9211=CARTESIAN_POINT('Origin',(-14.1,0.,5.));
#9212=CARTESIAN_POINT('',(-14.,-1.13892152320704E-16,5.93));
#9213=CARTESIAN_POINT('Origin',(-14.,0.,5.));
#9214=CARTESIAN_POINT('',(-14.1,-1.13892152320704E-16,5.93));
#9215=CARTESIAN_POINT('Origin',(-14.1,0.,5.));
#9216=CARTESIAN_POINT('',(-11.9,0.1,5.7836453279386));
#9217=CARTESIAN_POINT('Origin',(-12.,0.,5.));
#9218=CARTESIAN_POINT('',(-12.1,0.1,5.7836453279386));
#9219=CARTESIAN_POINT('',(-14.1,0.1,5.7836453279386));
#9220=CARTESIAN_POINT('Origin',(-12.,0.,5.));
#9221=CARTESIAN_POINT('',(-12.1,0.1,4.2163546720614));
#9222=CARTESIAN_POINT('Origin',(-12.,0.,5.));
#9223=CARTESIAN_POINT('',(-11.9,0.1,4.2163546720614));
#9224=CARTESIAN_POINT('',(-14.1,0.1,4.2163546720614));
#9225=CARTESIAN_POINT('Origin',(-12.,0.,5.));
#9226=CARTESIAN_POINT('Origin',(-12.,0.1,5.));
#9227=CARTESIAN_POINT('Origin',(-12.,0.1,5.));
#9228=CARTESIAN_POINT('Origin',(-12.,-2.1,5.));
#9229=CARTESIAN_POINT('Origin',(-12.,0.1,5.));
#9230=CARTESIAN_POINT('Origin',(-12.,-2.1,5.));
#9231=CARTESIAN_POINT('Origin',(-12.,0.1,5.));
#9232=CARTESIAN_POINT('Origin',(-12.,-2.,5.));
#9233=CARTESIAN_POINT('',(-12.,0.,6.6));
#9234=CARTESIAN_POINT('',(-12.,0.,3.4));
#9235=CARTESIAN_POINT('Origin',(-12.,0.,5.));
#9236=CARTESIAN_POINT('',(-13.6,-1.6,5.));
#9237=CARTESIAN_POINT('Origin',(-12.,0.,5.));
#9238=CARTESIAN_POINT('',(-13.6,-2.,5.));
#9239=CARTESIAN_POINT('',(-13.6,-2.,5.));
#9240=CARTESIAN_POINT('Origin',(-12.,-2.,5.));
#9241=CARTESIAN_POINT('Origin',(-12.,0.,5.));
#9242=CARTESIAN_POINT('Origin',(-12.,-2.,5.));
#9243=CARTESIAN_POINT('Origin',(-14.,0.,5.));
#9244=CARTESIAN_POINT('',(-10.,-1.95943487863577E-16,6.6));
#9245=CARTESIAN_POINT('Origin',(-10.,0.,5.));
#9246=CARTESIAN_POINT('',(-14.,-1.95943487863577E-16,6.6));
#9247=CARTESIAN_POINT('',(-14.,-1.95943487863577E-16,6.6));
#9248=CARTESIAN_POINT('',(-14.,-1.95943487863577E-16,6.6));
#9249=CARTESIAN_POINT('Origin',(-14.,0.,5.));
#9250=CARTESIAN_POINT('Origin',(-10.,0.,5.));
#9251=CARTESIAN_POINT('Origin',(-14.,0.,5.));
#9252=CARTESIAN_POINT('',(0.,0.,0.));
#9253=CARTESIAN_POINT('Origin',(-11.3,0.,5.));
#9254=CARTESIAN_POINT('',(-2.8,-9.67470971326409E-17,5.79));
#9255=CARTESIAN_POINT('Origin',(-2.8,0.,5.));
#9256=CARTESIAN_POINT('',(-11.3,-9.67470971326409E-17,5.79));
#9257=CARTESIAN_POINT('',(-11.3,-9.67470971326409E-17,5.79));
#9258=CARTESIAN_POINT('Origin',(-11.3,0.,5.));
#9259=CARTESIAN_POINT('Origin',(-11.3,0.,5.));
#9260=CARTESIAN_POINT('',(-2.8,-1.30424884109193E-16,6.065));
#9261=CARTESIAN_POINT('Origin',(-2.8,0.,5.));
#9262=CARTESIAN_POINT('',(-11.3,-1.30424884109193E-16,6.065));
#9263=CARTESIAN_POINT('',(-11.3,-1.30424884109193E-16,6.065));
#9264=CARTESIAN_POINT('Origin',(-11.3,0.,5.));
#9265=CARTESIAN_POINT('Origin',(-2.8,0.,5.));
#9266=CARTESIAN_POINT('Origin',(-11.3,0.,5.));
#9267=CARTESIAN_POINT('',(0.,0.,0.));
#9268=CARTESIAN_POINT('Origin',(-12.,-10.5,5.));
#9269=CARTESIAN_POINT('',(-12.79,-1.1,5.));
#9270=CARTESIAN_POINT('Origin',(-12.,-1.1,5.));
#9271=CARTESIAN_POINT('',(-12.79,-10.5,5.));
#9272=CARTESIAN_POINT('',(-12.79,-10.5,5.));
#9273=CARTESIAN_POINT('Origin',(-12.,-10.5,5.));
#9274=CARTESIAN_POINT('Origin',(-12.,-10.5,5.));
#9275=CARTESIAN_POINT('',(-13.065,-1.1,5.));
#9276=CARTESIAN_POINT('Origin',(-12.,-1.1,5.));
#9277=CARTESIAN_POINT('',(-13.065,-10.5,5.));
#9278=CARTESIAN_POINT('',(-13.065,-10.5,5.));
#9279=CARTESIAN_POINT('Origin',(-12.,-10.5,5.));
#9280=CARTESIAN_POINT('Origin',(-12.,-1.1,5.));
#9281=CARTESIAN_POINT('Origin',(-12.,-10.5,5.));
#9282=CARTESIAN_POINT('',(0.,0.,0.));
#9283=CARTESIAN_POINT('Origin',(-10.5,-12.,5.));
#9284=CARTESIAN_POINT('',(-1.8,-12.,5.79));
#9285=CARTESIAN_POINT('Origin',(-1.8,-12.,5.));
#9286=CARTESIAN_POINT('',(-10.5,-12.,5.79));
#9287=CARTESIAN_POINT('',(-10.5,-12.,5.79));
#9288=CARTESIAN_POINT('Origin',(-10.5,-12.,5.));
#9289=CARTESIAN_POINT('Origin',(-10.5,-12.,5.));
#9290=CARTESIAN_POINT('',(-1.8,-12.,6.065));
#9291=CARTESIAN_POINT('Origin',(-1.8,-12.,5.));
#9292=CARTESIAN_POINT('',(-10.5,-12.,6.065));
#9293=CARTESIAN_POINT('',(-10.5,-12.,6.065));
#9294=CARTESIAN_POINT('Origin',(-10.5,-12.,5.));
#9295=CARTESIAN_POINT('Origin',(-1.8,-12.,5.));
#9296=CARTESIAN_POINT('Origin',(-10.5,-12.,5.));
#9297=CARTESIAN_POINT('',(0.,0.,0.));
#9298=CARTESIAN_POINT('Origin',(0.,0.,0.));
#9299=CARTESIAN_POINT('',(0.276530287672074,0.276530287672074,0.740020945649513));
#9300=CARTESIAN_POINT('',(0.276530287672074,0.276530287672074,-0.740020945649513));
#9301=CARTESIAN_POINT('Origin',(0.,0.,0.));
#9302=CARTESIAN_POINT('',(-0.79,0.276530287672074,9.67470971326409E-17));
#9303=CARTESIAN_POINT('Origin',(0.,0.276530287672074,0.));
#9304=CARTESIAN_POINT('',(-0.79,1.45,-9.67470971326409E-17));
#9305=CARTESIAN_POINT('',(-0.79,0.,9.67470971326409E-17));
#9306=CARTESIAN_POINT('Origin',(0.,1.45,0.));
#9307=CARTESIAN_POINT('Origin',(0.,0.276530287672074,0.));
#9308=CARTESIAN_POINT('Origin',(0.,0.,0.));
#9309=CARTESIAN_POINT('',(-5.12514685443167E-17,-6.27649469043988E-33,-0.837));
#9310=CARTESIAN_POINT('',(-5.12514685443167E-17,-6.27649469043988E-33,0.837));
#9311=CARTESIAN_POINT('Origin',(0.,0.,0.));
#9312=CARTESIAN_POINT('',(0.276530287672074,-9.67470971326409E-17,0.79));
#9313=CARTESIAN_POINT('Origin',(0.276530287672074,0.,0.));
#9314=CARTESIAN_POINT('Origin',(0.276530287672074,0.,0.));
#9315=CARTESIAN_POINT('Origin',(0.,0.,0.));
#9316=CARTESIAN_POINT('',(1.45,9.67470971326409E-17,0.79));
#9317=CARTESIAN_POINT('',(0.,-9.67470971326409E-17,0.79));
#9318=CARTESIAN_POINT('Origin',(1.45,0.,0.));
#9319=CARTESIAN_POINT('Origin',(0.,1.45,0.));
#9320=CARTESIAN_POINT('',(-0.93,1.45,-1.13892152320704E-16));
#9321=CARTESIAN_POINT('Origin',(0.,1.45,0.));
#9322=CARTESIAN_POINT('Origin',(0.,2.175,0.));
#9323=CARTESIAN_POINT('',(-0.93,2.8,-1.13892152320704E-16));
#9324=CARTESIAN_POINT('Origin',(0.,2.8,0.));
#9325=CARTESIAN_POINT('',(-0.93,2.175,-1.13892152320704E-16));
#9326=CARTESIAN_POINT('Origin',(2.175,0.,0.));
#9327=CARTESIAN_POINT('',(1.45,-0.93,-1.13892152320704E-16));
#9328=CARTESIAN_POINT('Origin',(1.45,0.,0.));
#9329=CARTESIAN_POINT('',(2.8,-0.93,1.13892152320704E-16));
#9330=CARTESIAN_POINT('',(2.175,-0.93,-1.13892152320704E-16));
#9331=CARTESIAN_POINT('Origin',(2.8,0.,0.));
#9332=CARTESIAN_POINT('Origin',(1.45,0.93,0.));
#9333=CARTESIAN_POINT('Origin',(0.,0.,0.));
#9334=CARTESIAN_POINT('',(0.,0.,1.2));
#9335=CARTESIAN_POINT('',(-1.2,1.11022302462516E-16,-1.46957615897682E-16));
#9336=CARTESIAN_POINT('Origin',(0.,0.,0.));
#9337=CARTESIAN_POINT('',(0.,0.,-1.2));
#9338=CARTESIAN_POINT('Origin',(0.,0.,0.));
#9339=CARTESIAN_POINT('',(1.11022302462516E-16,-1.2,-1.46957615897682E-16));
#9340=CARTESIAN_POINT('Origin',(0.,0.,0.));
#9341=CARTESIAN_POINT('Origin',(0.,0.,0.));
#9342=CARTESIAN_POINT('Origin',(0.,0.9,0.));
#9343=CARTESIAN_POINT('Origin',(0.,0.,0.));
#9344=CARTESIAN_POINT('',(-1.2,1.8,-1.46957615897682E-16));
#9345=CARTESIAN_POINT('',(-1.2,0.9,-1.46957615897682E-16));
#9346=CARTESIAN_POINT('Origin',(0.,1.8,0.));
#9347=CARTESIAN_POINT('Origin',(1.45,2.8,0.));
#9348=CARTESIAN_POINT('',(-1.45,2.8,-1.77573785876366E-16));
#9349=CARTESIAN_POINT('Origin',(0.,2.8,0.));
#9350=CARTESIAN_POINT('Origin',(0.,2.3,0.));
#9351=CARTESIAN_POINT('',(-1.45,1.8,-1.77573785876366E-16));
#9352=CARTESIAN_POINT('Origin',(0.,1.8,0.));
#9353=CARTESIAN_POINT('',(-1.45,2.3,-1.77573785876366E-16));
#9354=CARTESIAN_POINT('Origin',(1.2,1.8,0.));
#9355=CARTESIAN_POINT('Origin',(1.8,1.45,0.));
#9356=CARTESIAN_POINT('',(1.8,-1.45,-1.77573785876366E-16));
#9357=CARTESIAN_POINT('Origin',(1.8,0.,0.));
#9358=CARTESIAN_POINT('',(1.8,-1.2,-1.46957615897682E-16));
#9359=CARTESIAN_POINT('Origin',(1.8,0.,0.));
#9360=CARTESIAN_POINT('Origin',(2.3,0.,0.));
#9361=CARTESIAN_POINT('',(2.8,-1.45,-1.77573785876366E-16));
#9362=CARTESIAN_POINT('Origin',(2.8,0.,0.));
#9363=CARTESIAN_POINT('',(2.3,-1.45,-1.77573785876366E-16));
#9364=CARTESIAN_POINT('Origin',(2.8,0.,0.));
#9365=CARTESIAN_POINT('Origin',(0.9,0.,0.));
#9366=CARTESIAN_POINT('',(0.9,-1.2,-1.46957615897682E-16));
#9367=CARTESIAN_POINT('',(0.,0.,0.));
#9368=CARTESIAN_POINT('Origin',(0.,-0.6,0.));
#9369=CARTESIAN_POINT('',(1.55884572681199,-0.6,0.));
#9370=CARTESIAN_POINT('',(0.779422863405995,-0.6,1.35));
#9371=CARTESIAN_POINT('',(0.779422863405995,-0.6,1.35));
#9372=CARTESIAN_POINT('',(-0.779422863405996,-0.6,1.35));
#9373=CARTESIAN_POINT('',(-0.779422863405996,-0.6,1.35));
#9374=CARTESIAN_POINT('',(-1.55884572681199,-0.6,-1.90903542970483E-16));
#9375=CARTESIAN_POINT('',(-1.55884572681199,-0.6,-1.90903542970483E-16));
#9376=CARTESIAN_POINT('',(-0.779422863405995,-0.6,-1.35));
#9377=CARTESIAN_POINT('',(-0.779422863405995,-0.6,-1.35));
#9378=CARTESIAN_POINT('',(0.779422863405995,-0.6,-1.35));
#9379=CARTESIAN_POINT('',(0.779422863405995,-0.6,-1.35));
#9380=CARTESIAN_POINT('',(1.55884572681199,-0.6,0.));
#9381=CARTESIAN_POINT('',(-1.065,-0.6,-1.30424884109193E-16));
#9382=CARTESIAN_POINT('Origin',(0.,-0.6,0.));
#9383=CARTESIAN_POINT('Origin',(0.,0.6,0.));
#9384=CARTESIAN_POINT('',(0.779422863405995,0.6,1.35));
#9385=CARTESIAN_POINT('',(1.55884572681199,0.6,0.));
#9386=CARTESIAN_POINT('',(0.779422863405995,0.6,1.35));
#9387=CARTESIAN_POINT('',(0.779422863405995,0.6,-1.35));
#9388=CARTESIAN_POINT('',(1.55884572681199,0.6,0.));
#9389=CARTESIAN_POINT('',(-0.779422863405995,0.6,-1.35));
#9390=CARTESIAN_POINT('',(0.779422863405995,0.6,-1.35));
#9391=CARTESIAN_POINT('',(-1.55884572681199,0.6,-1.90903542970483E-16));
#9392=CARTESIAN_POINT('',(-0.779422863405995,0.6,-1.35));
#9393=CARTESIAN_POINT('',(-0.779422863405996,0.6,1.35));
#9394=CARTESIAN_POINT('',(-1.55884572681199,0.6,-1.90903542970483E-16));
#9395=CARTESIAN_POINT('',(-0.779422863405996,0.6,1.35));
#9396=CARTESIAN_POINT('',(-1.065,0.6,1.30424884109193E-16));
#9397=CARTESIAN_POINT('Origin',(0.,0.6,0.));
#9398=CARTESIAN_POINT('Origin',(-0.779422863405996,0.,1.35));
#9399=CARTESIAN_POINT('',(0.779422863405995,0.,1.35));
#9400=CARTESIAN_POINT('',(-0.779422863405996,0.,1.35));
#9401=CARTESIAN_POINT('Origin',(-1.55884572681199,0.,-1.90903542970483E-16));
#9402=CARTESIAN_POINT('',(-1.55884572681199,0.,-1.90903542970483E-16));
#9403=CARTESIAN_POINT('Origin',(-0.779422863405995,0.,-1.35));
#9404=CARTESIAN_POINT('',(-0.779422863405995,0.,-1.35));
#9405=CARTESIAN_POINT('Origin',(0.779422863405995,0.,-1.35));
#9406=CARTESIAN_POINT('',(0.779422863405995,0.,-1.35));
#9407=CARTESIAN_POINT('Origin',(1.55884572681199,0.,0.));
#9408=CARTESIAN_POINT('',(1.55884572681199,0.,0.));
#9409=CARTESIAN_POINT('Origin',(0.779422863405995,0.,1.35));
#9410=CARTESIAN_POINT('Origin',(0.,0.,0.));
#9411=CARTESIAN_POINT('',(-1.065,2.47,-1.30424884109193E-16));
#9412=CARTESIAN_POINT('',(-1.065,0.,-1.30424884109193E-16));
#9413=CARTESIAN_POINT('Origin',(0.,2.47,0.));
#9414=CARTESIAN_POINT('Origin',(0.985,2.55,0.));
#9415=CARTESIAN_POINT('',(-0.985,2.55,-1.20627709716014E-16));
#9416=CARTESIAN_POINT('Origin',(0.,2.55,0.));
#9417=CARTESIAN_POINT('',(-0.79,2.55,-9.67470971326409E-17));
#9418=CARTESIAN_POINT('Origin',(0.,2.55,0.));
#9419=CARTESIAN_POINT('Origin',(0.,2.51,0.));
#9420=CARTESIAN_POINT('',(-1.025,2.51,-1.25526296912604E-16));
#9421=CARTESIAN_POINT('Origin',(0.,0.,0.));
#9422=CARTESIAN_POINT('',(-1.065,-2.47,-1.30424884109193E-16));
#9423=CARTESIAN_POINT('Origin',(0.,-2.47,0.));
#9424=CARTESIAN_POINT('',(-1.065,0.,-1.30424884109193E-16));
#9425=CARTESIAN_POINT('Origin',(0.,-2.51,0.));
#9426=CARTESIAN_POINT('',(-0.985,-2.55,-1.20627709716014E-16));
#9427=CARTESIAN_POINT('Origin',(0.,-2.55,0.));
#9428=CARTESIAN_POINT('',(-1.025,-2.51,-1.25526296912604E-16));
#9429=CARTESIAN_POINT('Origin',(0.79,-2.55,0.));
#9430=CARTESIAN_POINT('',(-0.79,-2.55,-9.67470971326409E-17));
#9431=CARTESIAN_POINT('Origin',(0.,-2.55,0.));
#9432=CARTESIAN_POINT('Origin',(0.,0.,0.));
#9433=CARTESIAN_POINT('',(-0.79,0.,-9.67470971326409E-17));
#9434=CARTESIAN_POINT('',(0.,0.,0.));
#9435=CARTESIAN_POINT('Origin',(-0.9,-1.90918830920368,4.09081169079632));
#9436=CARTESIAN_POINT('',(-0.8,-1.90918830920368,4.53081169079632));
#9437=CARTESIAN_POINT('Origin',(-0.8,-1.90918830920368,4.09081169079632));
#9438=CARTESIAN_POINT('',(-0.1,-1.90918830920368,4.53081169079632));
#9439=CARTESIAN_POINT('',(-0.9,-1.90918830920368,4.53081169079632));
#9440=CARTESIAN_POINT('Origin',(-0.1,-1.90918830920368,4.09081169079632));
#9441=CARTESIAN_POINT('Origin',(-0.9,-1.90918830920368,7.90918830920368));
#9442=CARTESIAN_POINT('',(-0.8,-1.90918830920368,8.34918830920368));
#9443=CARTESIAN_POINT('Origin',(-0.8,-1.90918830920368,7.90918830920368));
#9444=CARTESIAN_POINT('',(-0.1,-1.90918830920368,8.34918830920368));
#9445=CARTESIAN_POINT('',(-0.9,-1.90918830920368,8.34918830920368));
#9446=CARTESIAN_POINT('Origin',(-0.1,-1.90918830920368,7.90918830920368));
#9447=CARTESIAN_POINT('Origin',(-0.9,1.90918830920368,7.90918830920368));
#9448=CARTESIAN_POINT('',(-0.8,1.90918830920368,8.34918830920368));
#9449=CARTESIAN_POINT('Origin',(-0.8,1.90918830920368,7.90918830920368));
#9450=CARTESIAN_POINT('',(-0.1,1.90918830920368,8.34918830920368));
#9451=CARTESIAN_POINT('',(-0.9,1.90918830920368,8.34918830920368));
#9452=CARTESIAN_POINT('Origin',(-0.1,1.90918830920368,7.90918830920368));
#9453=CARTESIAN_POINT('Origin',(-0.9,1.90918830920368,4.09081169079632));
#9454=CARTESIAN_POINT('',(-0.8,1.90918830920368,4.53081169079632));
#9455=CARTESIAN_POINT('Origin',(-0.8,1.90918830920368,4.09081169079632));
#9456=CARTESIAN_POINT('',(-0.1,1.90918830920368,4.53081169079632));
#9457=CARTESIAN_POINT('',(-0.9,1.90918830920368,4.53081169079632));
#9458=CARTESIAN_POINT('Origin',(-0.1,1.90918830920368,4.09081169079632));
#9459=CARTESIAN_POINT('Origin',(-0.8,0.,6.));
#9460=CARTESIAN_POINT('',(-0.8,-4.28626379701574E-16,9.5));
#9461=CARTESIAN_POINT('Origin',(-0.8,0.,6.));
#9462=CARTESIAN_POINT('',(-0.8,1.83697019872103E-16,7.5));
#9463=CARTESIAN_POINT('Origin',(-0.8,0.,6.));
#9464=CARTESIAN_POINT('Origin',(-0.8,0.,6.));
#9465=CARTESIAN_POINT('',(-0.1,-4.28626379701574E-16,9.5));
#9466=CARTESIAN_POINT('Origin',(-0.1,0.,6.));
#9467=CARTESIAN_POINT('',(-0.8,-4.28626379701574E-16,9.5));
#9468=CARTESIAN_POINT('Origin',(-2.8,0.,6.));
#9469=CARTESIAN_POINT('',(-0.1,-9.67470971326409E-17,6.79));
#9470=CARTESIAN_POINT('Origin',(-0.1,0.,6.));
#9471=CARTESIAN_POINT('',(-2.8,-9.67470971326409E-17,6.79));
#9472=CARTESIAN_POINT('',(-2.8,-9.67470971326409E-17,6.79));
#9473=CARTESIAN_POINT('Origin',(-2.8,0.,6.));
#9474=CARTESIAN_POINT('Origin',(-2.8,0.,6.));
#9475=CARTESIAN_POINT('',(-2.8,-1.83697019872103E-16,7.5));
#9476=CARTESIAN_POINT('',(-2.8,-1.83697019872103E-16,7.5));
#9477=CARTESIAN_POINT('Origin',(-2.8,0.,6.));
#9478=CARTESIAN_POINT('Origin',(-0.1,0.,6.));
#9479=CARTESIAN_POINT('Origin',(-2.8,0.,6.));
#9480=CARTESIAN_POINT('',(0.,0.,0.));
#9481=CARTESIAN_POINT('Origin',(0.,-1.90918830920368,4.09081169079632));
#9482=CARTESIAN_POINT('',(0.1,-1.90918830920368,4.53081169079632));
#9483=CARTESIAN_POINT('Origin',(0.1,-1.90918830920368,4.09081169079632));
#9484=CARTESIAN_POINT('',(0.8,-1.90918830920368,4.53081169079632));
#9485=CARTESIAN_POINT('',(0.,-1.90918830920368,4.53081169079632));
#9486=CARTESIAN_POINT('Origin',(0.8,-1.90918830920368,4.09081169079632));
#9487=CARTESIAN_POINT('Origin',(0.,-1.90918830920368,7.90918830920368));
#9488=CARTESIAN_POINT('',(0.1,-1.90918830920368,8.34918830920368));
#9489=CARTESIAN_POINT('Origin',(0.1,-1.90918830920368,7.90918830920368));
#9490=CARTESIAN_POINT('',(0.8,-1.90918830920368,8.34918830920368));
#9491=CARTESIAN_POINT('',(0.,-1.90918830920368,8.34918830920368));
#9492=CARTESIAN_POINT('Origin',(0.8,-1.90918830920368,7.90918830920368));
#9493=CARTESIAN_POINT('Origin',(0.,1.90918830920368,7.90918830920368));
#9494=CARTESIAN_POINT('',(0.1,1.90918830920368,8.34918830920368));
#9495=CARTESIAN_POINT('Origin',(0.1,1.90918830920368,7.90918830920368));
#9496=CARTESIAN_POINT('',(0.8,1.90918830920368,8.34918830920368));
#9497=CARTESIAN_POINT('',(0.,1.90918830920368,8.34918830920368));
#9498=CARTESIAN_POINT('Origin',(0.8,1.90918830920368,7.90918830920368));
#9499=CARTESIAN_POINT('Origin',(0.,1.90918830920368,4.09081169079632));
#9500=CARTESIAN_POINT('',(0.1,1.90918830920368,4.53081169079632));
#9501=CARTESIAN_POINT('Origin',(0.1,1.90918830920368,4.09081169079632));
#9502=CARTESIAN_POINT('',(0.8,1.90918830920368,4.53081169079632));
#9503=CARTESIAN_POINT('',(0.,1.90918830920368,4.53081169079632));
#9504=CARTESIAN_POINT('Origin',(0.8,1.90918830920368,4.09081169079632));
#9505=CARTESIAN_POINT('Origin',(0.8,0.,6.));
#9506=CARTESIAN_POINT('',(0.8,-4.28626379701574E-16,9.5));
#9507=CARTESIAN_POINT('Origin',(0.8,0.,6.));
#9508=CARTESIAN_POINT('',(0.8,-1.83697019872103E-16,7.5));
#9509=CARTESIAN_POINT('Origin',(0.8,0.,6.));
#9510=CARTESIAN_POINT('Origin',(0.1,0.,6.));
#9511=CARTESIAN_POINT('',(0.1,-4.28626379701574E-16,9.5));
#9512=CARTESIAN_POINT('',(0.1,-4.28626379701574E-16,9.5));
#9513=CARTESIAN_POINT('Origin',(0.1,0.,6.));
#9514=CARTESIAN_POINT('Origin',(0.1,0.,6.));
#9515=CARTESIAN_POINT('',(2.8,-9.67470971326409E-17,6.79));
#9516=CARTESIAN_POINT('Origin',(2.8,0.,6.));
#9517=CARTESIAN_POINT('',(0.1,-9.67470971326409E-17,6.79));
#9518=CARTESIAN_POINT('',(0.1,-9.67470971326409E-17,6.79));
#9519=CARTESIAN_POINT('Origin',(0.1,0.,6.));
#9520=CARTESIAN_POINT('Origin',(0.1,0.,6.));
#9521=CARTESIAN_POINT('',(2.8,-1.83697019872103E-16,7.5));
#9522=CARTESIAN_POINT('Origin',(2.8,0.,6.));
#9523=CARTESIAN_POINT('',(0.1,-1.83697019872103E-16,7.5));
#9524=CARTESIAN_POINT('Origin',(2.8,0.,6.));
#9525=CARTESIAN_POINT('Origin',(0.1,0.,6.));
#9526=CARTESIAN_POINT('',(0.,0.,0.));
#9527=CARTESIAN_POINT('Origin',(0.6,0.8,0.));
#9528=CARTESIAN_POINT('',(-0.6,0.8,-7.34788079488412E-17));
#9529=CARTESIAN_POINT('Origin',(0.,0.8,0.));
#9530=CARTESIAN_POINT('Origin',(0.,0.775,0.));
#9531=CARTESIAN_POINT('',(-0.65,0.75,-7.9602041944578E-17));
#9532=CARTESIAN_POINT('Origin',(0.,0.75,0.));
#9533=CARTESIAN_POINT('',(-0.625,0.775,-7.65404249467096E-17));
#9534=CARTESIAN_POINT('Origin',(0.,0.39,0.));
#9535=CARTESIAN_POINT('',(-0.65,0.0299999999999998,-7.9602041944578E-17));
#9536=CARTESIAN_POINT('Origin',(0.,0.0299999999999998,0.));
#9537=CARTESIAN_POINT('',(-0.65,0.39,-7.9602041944578E-17));
#9538=CARTESIAN_POINT('Origin',(0.,0.0150000000000001,0.));
#9539=CARTESIAN_POINT('',(-0.62,5.89805981832114E-17,-7.59281015471359E-17));
#9540=CARTESIAN_POINT('Origin',(0.,0.,0.));
#9541=CARTESIAN_POINT('',(-0.635,0.0150000000000001,-7.77650717458569E-17));
#9542=CARTESIAN_POINT('Origin',(0.42,0.,0.));
#9543=CARTESIAN_POINT('',(-0.42,-3.46944695195361E-18,-5.14351655641888E-17));
#9544=CARTESIAN_POINT('Origin',(0.,0.,0.));
#9545=CARTESIAN_POINT('Origin',(0.,-0.02,0.));
#9546=CARTESIAN_POINT('',(-0.3933,-0.0534000000000001,4.81653586104654E-17));
#9547=CARTESIAN_POINT('Origin',(0.,-0.0534000000000001,0.));
#9548=CARTESIAN_POINT('',(-0.41,-0.02,-5.02105187650415E-17));
#9549=CARTESIAN_POINT('Origin',(0.,-1.48,0.));
#9550=CARTESIAN_POINT('',(-0.3933,-2.9267,4.81653586104654E-17));
#9551=CARTESIAN_POINT('Origin',(0.,-2.9267,0.));
#9552=CARTESIAN_POINT('',(-0.3933,-1.48,-4.81653586104654E-17));
#9553=CARTESIAN_POINT('Origin',(0.,-2.96,0.));
#9554=CARTESIAN_POINT('',(-0.32,-3.,-3.91886975727153E-17));
#9555=CARTESIAN_POINT('Origin',(0.,-3.,0.));
#9556=CARTESIAN_POINT('',(-0.36,-2.96,-4.40872847693047E-17));
#9557=CARTESIAN_POINT('Origin',(0.,-3.,0.));
#9558=CARTESIAN_POINT('Origin',(0.173205080756888,-0.8,-0.3));
#9559=CARTESIAN_POINT('',(0.346410161513775,-0.8,0.));
#9560=CARTESIAN_POINT('',(0.173205080756888,-0.8,-0.3));
#9561=CARTESIAN_POINT('',(0.346410161513775,-0.8,0.));
#9562=CARTESIAN_POINT('',(0.173205080756888,-1.28,-0.3));
#9563=CARTESIAN_POINT('',(0.173205080756888,-0.8,-0.3));
#9564=CARTESIAN_POINT('',(0.346410161513775,-1.28,0.));
#9565=CARTESIAN_POINT('',(0.346410161513775,-1.28,0.));
#9566=CARTESIAN_POINT('',(0.346410161513775,-0.8,0.));
#9567=CARTESIAN_POINT('Origin',(-0.173205080756888,-0.8,-0.3));
#9568=CARTESIAN_POINT('',(-0.173205080756888,-0.8,-0.3));
#9569=CARTESIAN_POINT('',(0.173205080756888,-0.8,-0.3));
#9570=CARTESIAN_POINT('',(-0.173205080756888,-1.28,-0.3));
#9571=CARTESIAN_POINT('',(-0.173205080756888,-0.8,-0.3));
#9572=CARTESIAN_POINT('',(0.173205080756888,-1.28,-0.3));
#9573=CARTESIAN_POINT('Origin',(-0.346410161513775,-0.8,-5.55111512312578E-17));
#9574=CARTESIAN_POINT('',(-0.346410161513775,-0.8,-4.24230095489963E-17));
#9575=CARTESIAN_POINT('',(-0.173205080756888,-0.8,-0.3));
#9576=CARTESIAN_POINT('',(-0.346410161513775,-1.28,-5.55111512312578E-17));
#9577=CARTESIAN_POINT('',(-0.346410161513775,-0.8,-4.24230095489963E-17));
#9578=CARTESIAN_POINT('',(-0.173205080756888,-1.28,-0.3));
#9579=CARTESIAN_POINT('Origin',(-0.173205080756888,-0.8,0.3));
#9580=CARTESIAN_POINT('',(-0.173205080756888,-0.8,0.3));
#9581=CARTESIAN_POINT('',(-0.346410161513775,-0.8,-4.24230095489963E-17));
#9582=CARTESIAN_POINT('',(-0.173205080756888,-1.28,0.3));
#9583=CARTESIAN_POINT('',(-0.173205080756888,-0.8,0.3));
#9584=CARTESIAN_POINT('',(-0.346410161513775,-1.28,-4.24230095489963E-17));
#9585=CARTESIAN_POINT('Origin',(0.173205080756888,-0.8,0.3));
#9586=CARTESIAN_POINT('',(0.173205080756888,-0.8,0.3));
#9587=CARTESIAN_POINT('',(-0.173205080756888,-0.8,0.3));
#9588=CARTESIAN_POINT('',(0.173205080756888,-1.28,0.3));
#9589=CARTESIAN_POINT('',(0.173205080756888,-0.8,0.3));
#9590=CARTESIAN_POINT('',(-0.173205080756888,-1.28,0.3));
#9591=CARTESIAN_POINT('Origin',(0.346410161513775,-0.8,0.));
#9592=CARTESIAN_POINT('',(0.173205080756888,-0.8,0.3));
#9593=CARTESIAN_POINT('',(0.173205080756888,-1.28,0.3));
#9594=CARTESIAN_POINT('Origin',(0.,-0.8,-5.55111512312578E-17));
#9595=CARTESIAN_POINT('Origin',(0.,-1.28,-5.55111512312578E-17));
#9596=CARTESIAN_POINT('',(0.,0.,0.));
#9597=CARTESIAN_POINT('Origin',(0.,0.,0.));
#9598=CARTESIAN_POINT('',(-0.42,0.16,5.14351655641888E-17));
#9599=CARTESIAN_POINT('Origin',(0.,0.16,0.));
#9600=CARTESIAN_POINT('',(-0.42,0.,5.14351655641888E-17));
#9601=CARTESIAN_POINT('',(-0.42,0.,5.14351655641888E-17));
#9602=CARTESIAN_POINT('Origin',(0.,0.,0.));
#9603=CARTESIAN_POINT('Origin',(0.,0.,0.));
#9604=CARTESIAN_POINT('',(-0.8,0.16,9.79717439317883E-17));
#9605=CARTESIAN_POINT('Origin',(0.,0.16,0.));
#9606=CARTESIAN_POINT('',(-0.8,0.,9.79717439317883E-17));
#9607=CARTESIAN_POINT('',(-0.8,0.,9.79717439317883E-17));
#9608=CARTESIAN_POINT('Origin',(0.,0.,0.));
#9609=CARTESIAN_POINT('Origin',(0.,0.16,0.));
#9610=CARTESIAN_POINT('Origin',(0.,0.,0.));
#9611=CARTESIAN_POINT('',(0.,0.,0.));
#9612=CARTESIAN_POINT('Origin',(0.,0.067277284513851,0.));
#9613=CARTESIAN_POINT('',(-0.375277674973257,0.0768195421087395,0.65));
#9614=CARTESIAN_POINT('',(0.375277674973257,0.0768195421087395,0.65));
#9615=CARTESIAN_POINT('Ctrl Pts',(-0.375277674973257,0.0768195421087395,
0.65));
#9616=CARTESIAN_POINT('Ctrl Pts',(1.66533453693773E-13,-0.0315137912242439,
0.65));
#9617=CARTESIAN_POINT('Ctrl Pts',(0.375277674973257,0.0768195421087394,
0.65));
#9618=CARTESIAN_POINT('',(-0.750555349946514,0.0768195421087394,-9.19165206894919E-17));
#9619=CARTESIAN_POINT('Ctrl Pts',(-0.750555349946514,0.0768195421087394,
-9.19165206894919E-17));
#9620=CARTESIAN_POINT('Ctrl Pts',(-0.562916512459802,-0.0315137912242434,
0.325000000000144));
#9621=CARTESIAN_POINT('Ctrl Pts',(-0.375277674973257,0.0768195421087395,
0.65));
#9622=CARTESIAN_POINT('',(-0.6175,-2.77555756156289E-17,-7.5621939847349E-17));
#9623=CARTESIAN_POINT('',(-0.734027674973257,0.067277284513851,-8.98924642641573E-17));
#9624=CARTESIAN_POINT('Origin',(0.,0.,0.));
#9625=CARTESIAN_POINT('',(-0.375277674973257,0.0768195421087395,-0.65));
#9626=CARTESIAN_POINT('Ctrl Pts',(-0.375277674973257,0.0768195421087395,
-0.65));
#9627=CARTESIAN_POINT('Ctrl Pts',(-0.562916512459968,-0.0315137912242437,
-0.324999999999856));
#9628=CARTESIAN_POINT('Ctrl Pts',(-0.750555349946514,0.0768195421087395,
-9.19165206894919E-17));
#9629=CARTESIAN_POINT('',(0.375277674973257,0.0768195421087395,-0.65));
#9630=CARTESIAN_POINT('Ctrl Pts',(0.375277674973257,0.0768195421087395,
-0.65));
#9631=CARTESIAN_POINT('Ctrl Pts',(-1.66144875635155E-13,-0.0315137912242437,
-0.65));
#9632=CARTESIAN_POINT('Ctrl Pts',(-0.375277674973257,0.0768195421087395,
-0.65));
#9633=CARTESIAN_POINT('',(0.750555349946514,0.0768195421087394,0.));
#9634=CARTESIAN_POINT('Ctrl Pts',(0.750555349946514,0.0768195421087394,
0.));
#9635=CARTESIAN_POINT('Ctrl Pts',(0.562916512459802,-0.0315137912242436,
-0.325000000000144));
#9636=CARTESIAN_POINT('Ctrl Pts',(0.375277674973257,0.0768195421087395,
-0.65));
#9637=CARTESIAN_POINT('Ctrl Pts',(0.375277674973257,0.0768195421087394,
0.65));
#9638=CARTESIAN_POINT('Ctrl Pts',(0.562916512459968,-0.0315137912242439,
0.324999999999856));
#9639=CARTESIAN_POINT('Ctrl Pts',(0.750555349946514,0.0768195421087394,
0.));
#9640=CARTESIAN_POINT('Origin',(0.,0.612722715486149,0.));
#9641=CARTESIAN_POINT('',(-0.6175,0.68,-7.5621939847349E-17));
#9642=CARTESIAN_POINT('Origin',(0.,0.68,0.));
#9643=CARTESIAN_POINT('',(-0.750555349946514,0.603180457891261,-9.19165206894919E-17));
#9644=CARTESIAN_POINT('',(-0.734027674973257,0.612722715486149,-8.98924642641573E-17));
#9645=CARTESIAN_POINT('',(-0.375277674973257,0.603180457891261,0.65));
#9646=CARTESIAN_POINT('Ctrl Pts',(-0.375277674973257,0.603180457891261,
0.65));
#9647=CARTESIAN_POINT('Ctrl Pts',(-0.562916512459968,0.711513791224243,
0.324999999999856));
#9648=CARTESIAN_POINT('Ctrl Pts',(-0.750555349946514,0.603180457891261,
-9.19165206894919E-17));
#9649=CARTESIAN_POINT('',(0.375277674973257,0.603180457891261,0.65));
#9650=CARTESIAN_POINT('Ctrl Pts',(0.375277674973257,0.603180457891261,0.65));
#9651=CARTESIAN_POINT('Ctrl Pts',(-1.66755498298699E-13,0.711513791224244,
0.65));
#9652=CARTESIAN_POINT('Ctrl Pts',(-0.375277674973257,0.603180457891261,
0.65));
#9653=CARTESIAN_POINT('',(0.750555349946514,0.603180457891261,0.));
#9654=CARTESIAN_POINT('Ctrl Pts',(0.750555349946514,0.603180457891261,0.));
#9655=CARTESIAN_POINT('Ctrl Pts',(0.562916512459802,0.711513791224244,0.325000000000144));
#9656=CARTESIAN_POINT('Ctrl Pts',(0.375277674973257,0.603180457891261,0.65));
#9657=CARTESIAN_POINT('',(0.375277674973257,0.603180457891261,-0.65));
#9658=CARTESIAN_POINT('Ctrl Pts',(0.375277674973257,0.603180457891261,-0.65));
#9659=CARTESIAN_POINT('Ctrl Pts',(0.562916512459969,0.711513791224244,-0.324999999999856));
#9660=CARTESIAN_POINT('Ctrl Pts',(0.750555349946514,0.603180457891261,0.));
#9661=CARTESIAN_POINT('',(-0.375277674973257,0.603180457891261,-0.65));
#9662=CARTESIAN_POINT('Ctrl Pts',(-0.375277674973257,0.603180457891261,
-0.65));
#9663=CARTESIAN_POINT('Ctrl Pts',(1.66422431391311E-13,0.711513791224244,
-0.65));
#9664=CARTESIAN_POINT('Ctrl Pts',(0.375277674973257,0.603180457891261,-0.65));
#9665=CARTESIAN_POINT('Ctrl Pts',(-0.750555349946514,0.603180457891261,
-9.19165206894919E-17));
#9666=CARTESIAN_POINT('Ctrl Pts',(-0.562916512459802,0.711513791224244,
-0.325000000000144));
#9667=CARTESIAN_POINT('Ctrl Pts',(-0.375277674973257,0.603180457891261,
-0.65));
#9668=CARTESIAN_POINT('Origin',(0.375277674973257,0.,-0.65));
#9669=CARTESIAN_POINT('',(-0.375277674973257,0.,-0.65));
#9670=CARTESIAN_POINT('',(0.375277674973257,0.,-0.65));
#9671=CARTESIAN_POINT('Origin',(-0.375277674973257,0.,-0.65));
#9672=CARTESIAN_POINT('',(-0.750555349946514,0.,-9.19165206894919E-17));
#9673=CARTESIAN_POINT('Origin',(-0.750555349946514,0.,-9.19165206894919E-17));
#9674=CARTESIAN_POINT('',(-0.375277674973257,0.,0.65));
#9675=CARTESIAN_POINT('Origin',(0.,0.,0.));
#9676=CARTESIAN_POINT('',(-0.338975,0.68,4.15124648740974E-17));
#9677=CARTESIAN_POINT('Origin',(0.,0.68,0.));
#9678=CARTESIAN_POINT('',(-0.338975,0.,4.15124648740974E-17));
#9679=CARTESIAN_POINT('',(-0.338975,0.,4.15124648740974E-17));
#9680=CARTESIAN_POINT('Origin',(0.,0.,0.));
#9681=CARTESIAN_POINT('Origin',(-0.375277674973257,0.,0.65));
#9682=CARTESIAN_POINT('',(0.375277674973257,0.,0.65));
#9683=CARTESIAN_POINT('Origin',(0.750555349946514,0.,0.));
#9684=CARTESIAN_POINT('',(0.750555349946514,0.,0.));
#9685=CARTESIAN_POINT('Origin',(0.375277674973257,0.,0.65));
#9686=CARTESIAN_POINT('Origin',(0.,0.68,-1.11022302462516E-16));
#9687=CARTESIAN_POINT('Origin',(0.,0.,-1.11022302462516E-16));
#9688=CARTESIAN_POINT('',(0.,-12.,0.));
#9689=CARTESIAN_POINT('',(0.,0.,-1.));
#9690=CARTESIAN_POINT('',(0.,0.,0.));
#9691=CARTESIAN_POINT('',(0.,0.,0.));
#9692=CARTESIAN_POINT('',(0.,0.,0.));
#9693=CARTESIAN_POINT('',(0.,0.,0.));
#9694=CARTESIAN_POINT('',(24.,0.,0.));
#9695=CARTESIAN_POINT('',(0.,0.,0.));
#9696=CARTESIAN_POINT('',(24.,0.,0.));
#9697=CARTESIAN_POINT('',(0.,-24.,0.));
#9698=CARTESIAN_POINT('',(-12.,-12.,5.));
#9699=CARTESIAN_POINT('',(12.,-12.,5.));
#9700=CARTESIAN_POINT('',(-15.35,0.,5.));
#9701=CARTESIAN_POINT('',(15.35,0.,5.));
#9702=CARTESIAN_POINT('',(0.,0.,-1.));
#9703=CARTESIAN_POINT('',(0.,0.,-1.));
#9704=CARTESIAN_POINT('',(-0.96,1.90918830920368,6.90918830920368));
#9705=CARTESIAN_POINT('',(-0.96,1.90918830920368,6.90918830920368));
#9706=CARTESIAN_POINT('',(0.8,1.90918830920368,6.90918830920368));
#9707=CARTESIAN_POINT('',(0.96,1.90918830920368,6.90918830920368));
#9708=CARTESIAN_POINT('',(-0.96,-1.90918830920368,6.90918830920368));
#9709=CARTESIAN_POINT('',(-0.96,-1.90918830920368,6.90918830920368));
#9710=CARTESIAN_POINT('',(0.8,-1.90918830920368,6.90918830920368));
#9711=CARTESIAN_POINT('',(0.96,-1.90918830920368,6.90918830920368));
#9712=CARTESIAN_POINT('',(-0.96,-1.90918830920368,3.09081169079632));
#9713=CARTESIAN_POINT('',(-0.96,-1.90918830920368,3.09081169079632));
#9714=CARTESIAN_POINT('',(0.8,-1.90918830920368,3.09081169079632));
#9715=CARTESIAN_POINT('',(0.96,-1.90918830920368,3.09081169079632));
#9716=CARTESIAN_POINT('',(-0.96,1.90918830920368,3.09081169079632));
#9717=CARTESIAN_POINT('',(-0.96,1.90918830920368,3.09081169079632));
#9718=CARTESIAN_POINT('',(0.8,1.90918830920368,3.09081169079632));
#9719=CARTESIAN_POINT('',(0.96,1.90918830920368,3.09081169079632));
#9720=CARTESIAN_POINT('',(0.,0.,0.));
#9721=CARTESIAN_POINT('',(0.,0.,0.));
#9722=CARTESIAN_POINT('Origin',(-0.205,-0.205,6.));
#9723=CARTESIAN_POINT('',(0.205,-0.205,6.47171668469172));
#9724=CARTESIAN_POINT('',(-0.205,-0.205,6.47171668469172));
#9725=CARTESIAN_POINT('Origin',(0.,-0.205,5.));
#9726=CARTESIAN_POINT('',(0.205,-0.205,6.));
#9727=CARTESIAN_POINT('',(0.205,-0.205,6.));
#9728=CARTESIAN_POINT('',(-0.205,-0.205,6.));
#9729=CARTESIAN_POINT('',(-0.205,-0.205,6.));
#9730=CARTESIAN_POINT('',(-0.205,-0.205,6.));
#9731=CARTESIAN_POINT('Origin',(-0.205,0.205,6.));
#9732=CARTESIAN_POINT('',(-0.205,-2.51052593825207E-17,6.48592563743951));
#9733=CARTESIAN_POINT('Origin',(-0.205,0.,5.));
#9734=CARTESIAN_POINT('',(-0.205,0.205,6.));
#9735=CARTESIAN_POINT('',(-0.205,0.205,6.));
#9736=CARTESIAN_POINT('',(-0.205,0.205,6.47171668469172));
#9737=CARTESIAN_POINT('',(-0.205,0.205,6.));
#9738=CARTESIAN_POINT('Origin',(-0.205,0.,5.));
#9739=CARTESIAN_POINT('Origin',(0.205,0.205,6.));
#9740=CARTESIAN_POINT('',(0.205,0.205,6.47171668469172));
#9741=CARTESIAN_POINT('Origin',(0.,0.205,5.));
#9742=CARTESIAN_POINT('',(0.205,0.205,6.));
#9743=CARTESIAN_POINT('',(0.205,0.205,6.));
#9744=CARTESIAN_POINT('',(0.205,0.205,6.));
#9745=CARTESIAN_POINT('Origin',(0.205,-0.205,6.));
#9746=CARTESIAN_POINT('Origin',(0.205,0.,5.));
#9747=CARTESIAN_POINT('',(0.205,-0.205,6.));
#9748=CARTESIAN_POINT('Origin',(0.,0.,6.));
#9749=CARTESIAN_POINT('Origin',(0.,-1.6,5.));
#9750=CARTESIAN_POINT('',(-0.75,-1.29903810567666,5.));
#9751=CARTESIAN_POINT('Origin',(0.,-1.29903810567666,5.));
#9752=CARTESIAN_POINT('',(-0.75,1.29903810567666,5.));
#9753=CARTESIAN_POINT('',(-0.75,-1.6,5.));
#9754=CARTESIAN_POINT('Origin',(0.,1.29903810567666,5.));
#9755=CARTESIAN_POINT('Origin',(0.,0.,5.));
#9756=CARTESIAN_POINT('',(-9.18485099360515E-17,-1.12481983699639E-32,3.5));
#9757=CARTESIAN_POINT('Origin',(0.,0.,5.));
#9758=CARTESIAN_POINT('',(0.,0.,0.));
#9759=CARTESIAN_POINT('Origin',(0.,0.,8.5));
#9760=CARTESIAN_POINT('',(-0.165,-2.02066721859313E-17,8.5));
#9761=CARTESIAN_POINT('Origin',(0.,0.,8.5));
#9762=CARTESIAN_POINT('',(-0.165,2.02066721859313E-17,9.4));
#9763=CARTESIAN_POINT('',(-0.165,-2.02066721859313E-17,8.5));
#9764=CARTESIAN_POINT('Origin',(0.,0.,9.4));
#9765=CARTESIAN_POINT('Origin',(0.,0.,8.5));
#9766=CARTESIAN_POINT('Origin',(0.,0.,8.7));
#9767=CARTESIAN_POINT('',(-0.264575131106459,0.3,8.7));
#9768=CARTESIAN_POINT('',(-0.3,0.264575131106459,8.7));
#9769=CARTESIAN_POINT('Origin',(0.,0.,8.7));
#9770=CARTESIAN_POINT('',(-0.3,0.3,8.7));
#9771=CARTESIAN_POINT('',(-0.3,0.3,8.7));
#9772=CARTESIAN_POINT('',(0.3,0.3,8.7));
#9773=CARTESIAN_POINT('Origin',(0.,0.,8.7));
#9774=CARTESIAN_POINT('',(-0.3,-0.264575131106459,8.7));
#9775=CARTESIAN_POINT('',(-0.264575131106459,-0.3,8.7));
#9776=CARTESIAN_POINT('Origin',(0.,0.,8.7));
#9777=CARTESIAN_POINT('',(-0.3,-0.3,8.7));
#9778=CARTESIAN_POINT('',(-0.3,-0.3,8.7));
#9779=CARTESIAN_POINT('',(-0.3,0.3,8.7));
#9780=CARTESIAN_POINT('Origin',(0.,0.,8.7));
#9781=CARTESIAN_POINT('',(0.264575131106459,-0.3,8.7));
#9782=CARTESIAN_POINT('',(0.3,-0.264575131106459,8.7));
#9783=CARTESIAN_POINT('Origin',(0.,0.,8.7));
#9784=CARTESIAN_POINT('',(0.3,-0.3,8.7));
#9785=CARTESIAN_POINT('',(0.3,-0.3,8.7));
#9786=CARTESIAN_POINT('',(-0.3,-0.3,8.7));
#9787=CARTESIAN_POINT('Origin',(0.,0.,8.7));
#9788=CARTESIAN_POINT('',(0.3,0.264575131106459,8.7));
#9789=CARTESIAN_POINT('',(0.264575131106459,0.3,8.7));
#9790=CARTESIAN_POINT('Origin',(0.,0.,8.7));
#9791=CARTESIAN_POINT('',(0.3,0.3,8.7));
#9792=CARTESIAN_POINT('',(0.3,0.3,8.7));
#9793=CARTESIAN_POINT('',(0.3,-0.3,8.7));
#9794=CARTESIAN_POINT('Origin',(0.3,0.3,8.7));
#9795=CARTESIAN_POINT('',(0.15,0.3,8.7));
#9796=CARTESIAN_POINT('',(-0.3,0.3,9.4));
#9797=CARTESIAN_POINT('',(-0.3,0.3,8.7));
#9798=CARTESIAN_POINT('',(0.3,0.3,9.4));
#9799=CARTESIAN_POINT('',(0.3,0.3,9.4));
#9800=CARTESIAN_POINT('',(0.3,0.3,8.7));
#9801=CARTESIAN_POINT('Origin',(0.3,-0.3,8.7));
#9802=CARTESIAN_POINT('',(0.3,-0.15,8.7));
#9803=CARTESIAN_POINT('',(0.3,-0.3,9.4));
#9804=CARTESIAN_POINT('',(0.3,-0.3,9.4));
#9805=CARTESIAN_POINT('',(0.3,-0.3,8.7));
#9806=CARTESIAN_POINT('Origin',(-0.3,-0.3,8.7));
#9807=CARTESIAN_POINT('',(-0.15,-0.3,8.7));
#9808=CARTESIAN_POINT('',(-0.3,-0.3,9.4));
#9809=CARTESIAN_POINT('',(-0.3,-0.3,9.4));
#9810=CARTESIAN_POINT('',(-0.3,-0.3,8.7));
#9811=CARTESIAN_POINT('Origin',(-0.3,0.3,8.7));
#9812=CARTESIAN_POINT('',(-0.3,0.15,8.7));
#9813=CARTESIAN_POINT('',(-0.3,0.3,9.4));
#9814=CARTESIAN_POINT('Origin',(0.,0.,9.4));
#9815=CARTESIAN_POINT('Origin',(0.,0.,8.7));
#9816=CARTESIAN_POINT('Origin',(0.,0.,8.7));
#9817=CARTESIAN_POINT('Origin',(0.,0.,8.7));
#9818=CARTESIAN_POINT('',(-0.4,-4.89858719658941E-17,8.7));
#9819=CARTESIAN_POINT('Origin',(0.,0.,8.7));
#9820=CARTESIAN_POINT('Origin',(0.,0.,8.7));
#9821=CARTESIAN_POINT('Origin',(0.,0.,8.7));
#9822=CARTESIAN_POINT('Origin',(0.,0.,8.7));
#9823=CARTESIAN_POINT('Origin',(0.,0.,8.7));
#9824=CARTESIAN_POINT('Origin',(0.,0.,8.7));
#9825=CARTESIAN_POINT('Origin',(0.2,0.2,6.));
#9826=CARTESIAN_POINT('',(0.2,0.2,6.));
#9827=CARTESIAN_POINT('',(-0.2,0.2,6.));
#9828=CARTESIAN_POINT('',(0.2,0.2,6.));
#9829=CARTESIAN_POINT('',(-0.2,0.2,6.5));
#9830=CARTESIAN_POINT('',(-0.2,0.2,6.));
#9831=CARTESIAN_POINT('',(0.2,0.2,6.5));
#9832=CARTESIAN_POINT('',(0.1,0.2,6.5));
#9833=CARTESIAN_POINT('',(0.2,0.2,6.));
#9834=CARTESIAN_POINT('Origin',(0.2,-0.2,6.));
#9835=CARTESIAN_POINT('',(0.2,-0.2,6.));
#9836=CARTESIAN_POINT('',(0.2,-0.2,6.));
#9837=CARTESIAN_POINT('',(0.2,-0.2,6.5));
#9838=CARTESIAN_POINT('',(0.2,-0.1,6.5));
#9839=CARTESIAN_POINT('',(0.2,-0.2,6.));
#9840=CARTESIAN_POINT('Origin',(-0.2,-0.2,6.));
#9841=CARTESIAN_POINT('',(-0.2,-0.2,6.));
#9842=CARTESIAN_POINT('',(-0.2,-0.2,6.));
#9843=CARTESIAN_POINT('',(-0.2,-0.2,6.5));
#9844=CARTESIAN_POINT('',(-0.1,-0.2,6.5));
#9845=CARTESIAN_POINT('',(-0.2,-0.2,6.));
#9846=CARTESIAN_POINT('Origin',(-0.2,0.2,6.));
#9847=CARTESIAN_POINT('',(-0.2,0.2,6.));
#9848=CARTESIAN_POINT('',(-0.2,0.1,6.5));
#9849=CARTESIAN_POINT('Origin',(0.,0.,6.));
#9850=CARTESIAN_POINT('Origin',(0.,0.,6.5));
#9851=CARTESIAN_POINT('',(-0.4,-4.89858719658941E-17,6.5));
#9852=CARTESIAN_POINT('',(-0.4,-4.89858719658941E-17,6.5));
#9853=CARTESIAN_POINT('Origin',(0.,0.,6.5));
#9854=CARTESIAN_POINT('Origin',(0.,0.,6.5));
#9855=CARTESIAN_POINT('',(0.,0.,0.));
#9856=CARTESIAN_POINT('Origin',(-0.305,-0.305,8.9));
#9857=CARTESIAN_POINT('',(0.305,-0.305,9.4));
#9858=CARTESIAN_POINT('',(-0.305,-0.305,9.4));
#9859=CARTESIAN_POINT('',(1.6475,-0.305,9.4));
#9860=CARTESIAN_POINT('',(0.305,-0.305,9.));
#9861=CARTESIAN_POINT('',(0.305,-0.305,8.9));
#9862=CARTESIAN_POINT('',(-0.305,-0.305,9.));
#9863=CARTESIAN_POINT('',(1.6475,-0.305,9.));
#9864=CARTESIAN_POINT('',(-0.305,-0.305,8.9));
#9865=CARTESIAN_POINT('Origin',(-0.305,0.305,8.9));
#9866=CARTESIAN_POINT('',(-0.305,0.305,9.4));
#9867=CARTESIAN_POINT('',(-0.305,0.1525,9.4));
#9868=CARTESIAN_POINT('',(-0.305,0.305,9.));
#9869=CARTESIAN_POINT('',(-0.305,0.1525,9.));
#9870=CARTESIAN_POINT('',(-0.305,0.305,8.9));
#9871=CARTESIAN_POINT('Origin',(0.305,0.305,8.9));
#9872=CARTESIAN_POINT('',(0.305,0.305,9.4));
#9873=CARTESIAN_POINT('',(1.9525,0.305,9.4));
#9874=CARTESIAN_POINT('',(0.305,0.305,9.));
#9875=CARTESIAN_POINT('',(1.9525,0.305,9.));
#9876=CARTESIAN_POINT('',(0.305,0.305,8.9));
#9877=CARTESIAN_POINT('Origin',(0.305,-0.305,8.9));
#9878=CARTESIAN_POINT('',(0.305,-0.1525,9.4));
#9879=CARTESIAN_POINT('',(0.305,-0.1525,9.));
#9880=CARTESIAN_POINT('Origin',(8.,0.8,9.));
#9881=CARTESIAN_POINT('',(8.,0.8,9.));
#9882=CARTESIAN_POINT('',(-0.8,0.8,9.));
#9883=CARTESIAN_POINT('',(8.,0.8,9.));
#9884=CARTESIAN_POINT('',(-0.8,0.8,9.4));
#9885=CARTESIAN_POINT('',(-0.8,0.8,9.));
#9886=CARTESIAN_POINT('',(8.,0.8,9.4));
#9887=CARTESIAN_POINT('',(8.,0.8,9.4));
#9888=CARTESIAN_POINT('',(8.,0.8,9.));
#9889=CARTESIAN_POINT('Origin',(8.,-0.8,9.));
#9890=CARTESIAN_POINT('',(8.,-0.8,9.));
#9891=CARTESIAN_POINT('',(8.,-0.8,9.));
#9892=CARTESIAN_POINT('',(8.,-0.8,9.4));
#9893=CARTESIAN_POINT('',(8.,-0.8,9.4));
#9894=CARTESIAN_POINT('',(8.,-0.8,9.));
#9895=CARTESIAN_POINT('Origin',(-0.8,-0.8,9.));
#9896=CARTESIAN_POINT('',(-0.8,-0.8,9.));
#9897=CARTESIAN_POINT('',(-0.8,-0.8,9.));
#9898=CARTESIAN_POINT('',(-0.8,-0.8,9.4));
#9899=CARTESIAN_POINT('',(-0.8,-0.8,9.4));
#9900=CARTESIAN_POINT('',(-0.8,-0.8,9.));
#9901=CARTESIAN_POINT('Origin',(-0.8,0.8,9.));
#9902=CARTESIAN_POINT('',(-0.8,0.8,9.));
#9903=CARTESIAN_POINT('',(-0.8,0.8,9.4));
#9904=CARTESIAN_POINT('Origin',(3.6,0.,9.4));
#9905=CARTESIAN_POINT('Origin',(3.6,0.,9.));
#9906=CARTESIAN_POINT('',(0.,0.,0.));
#9907=CARTESIAN_POINT('Origin',(0.,0.,9.4));
#9908=CARTESIAN_POINT('',(-0.225,-2.75545529808154E-17,9.6));
#9909=CARTESIAN_POINT('Origin',(0.,0.,9.6));
#9910=CARTESIAN_POINT('',(-0.225,-2.75545529808154E-17,9.4));
#9911=CARTESIAN_POINT('',(-0.225,-2.75545529808154E-17,9.4));
#9912=CARTESIAN_POINT('Origin',(0.,0.,9.4));
#9913=CARTESIAN_POINT('Origin',(0.,0.,9.4));
#9914=CARTESIAN_POINT('',(-0.6,-7.34788079488412E-17,9.6));
#9915=CARTESIAN_POINT('Origin',(0.,0.,9.6));
#9916=CARTESIAN_POINT('',(-0.6,-7.34788079488412E-17,9.4));
#9917=CARTESIAN_POINT('',(-0.6,-7.34788079488412E-17,9.4));
#9918=CARTESIAN_POINT('Origin',(0.,0.,9.4));
#9919=CARTESIAN_POINT('Origin',(0.,0.,9.6));
#9920=CARTESIAN_POINT('Origin',(0.,0.,9.4));
#9921=CARTESIAN_POINT('',(0.,0.,0.));
#9922=CARTESIAN_POINT('Origin',(8.5,1.,9.4));
#9923=CARTESIAN_POINT('',(8.5,1.,9.4));
#9924=CARTESIAN_POINT('',(6.,1.,9.4));
#9925=CARTESIAN_POINT('',(8.5,1.,9.4));
#9926=CARTESIAN_POINT('',(6.,1.,10.2));
#9927=CARTESIAN_POINT('',(6.,1.,9.4));
#9928=CARTESIAN_POINT('',(8.5,1.,10.2));
#9929=CARTESIAN_POINT('',(8.5,1.,10.2));
#9930=CARTESIAN_POINT('',(8.5,1.,9.4));
#9931=CARTESIAN_POINT('Origin',(8.5,-1.,9.4));
#9932=CARTESIAN_POINT('',(8.5,-1.,9.4));
#9933=CARTESIAN_POINT('',(8.5,-1.,9.4));
#9934=CARTESIAN_POINT('',(8.5,-1.,10.2));
#9935=CARTESIAN_POINT('',(8.5,-1.,10.2));
#9936=CARTESIAN_POINT('',(8.5,-1.,9.4));
#9937=CARTESIAN_POINT('Origin',(6.,-1.,9.4));
#9938=CARTESIAN_POINT('',(6.,-1.,9.4));
#9939=CARTESIAN_POINT('',(6.,-1.,9.4));
#9940=CARTESIAN_POINT('',(6.,-1.,10.2));
#9941=CARTESIAN_POINT('',(6.,-1.,10.2));
#9942=CARTESIAN_POINT('',(6.,-1.,9.4));
#9943=CARTESIAN_POINT('Origin',(6.,1.,9.4));
#9944=CARTESIAN_POINT('',(6.,1.,9.4));
#9945=CARTESIAN_POINT('',(6.,1.,10.2));
#9946=CARTESIAN_POINT('Origin',(7.25,0.,10.2));
#9947=CARTESIAN_POINT('Origin',(7.25,0.,9.4));
#9948=CARTESIAN_POINT('',(0.,0.,0.));
#9949=CARTESIAN_POINT('Origin',(0.0866025403784439,-0.4,-0.15));
#9950=CARTESIAN_POINT('',(0.173205080756888,-0.4,0.));
#9951=CARTESIAN_POINT('',(0.0866025403784439,-0.4,-0.15));
#9952=CARTESIAN_POINT('',(0.173205080756888,-0.4,0.));
#9953=CARTESIAN_POINT('',(0.0866025403784439,-0.64,-0.15));
#9954=CARTESIAN_POINT('',(0.0866025403784439,-0.4,-0.15));
#9955=CARTESIAN_POINT('',(0.173205080756888,-0.64,0.));
#9956=CARTESIAN_POINT('',(0.173205080756888,-0.64,0.));
#9957=CARTESIAN_POINT('',(0.173205080756888,-0.4,0.));
#9958=CARTESIAN_POINT('Origin',(-0.0866025403784438,-0.4,-0.15));
#9959=CARTESIAN_POINT('',(-0.0866025403784438,-0.4,-0.15));
#9960=CARTESIAN_POINT('',(0.0866025403784439,-0.4,-0.15));
#9961=CARTESIAN_POINT('',(-0.0866025403784438,-0.64,-0.15));
#9962=CARTESIAN_POINT('',(-0.0866025403784438,-0.4,-0.15));
#9963=CARTESIAN_POINT('',(0.0866025403784439,-0.64,-0.15));
#9964=CARTESIAN_POINT('Origin',(-0.173205080756888,-0.4,-2.77555756156289E-17));
#9965=CARTESIAN_POINT('',(-0.173205080756888,-0.4,-2.12115047744981E-17));
#9966=CARTESIAN_POINT('',(-0.0866025403784438,-0.4,-0.15));
#9967=CARTESIAN_POINT('',(-0.173205080756888,-0.64,-2.77555756156289E-17));
#9968=CARTESIAN_POINT('',(-0.173205080756888,-0.4,-2.12115047744981E-17));
#9969=CARTESIAN_POINT('',(-0.0866025403784438,-0.64,-0.15));
#9970=CARTESIAN_POINT('Origin',(-0.0866025403784439,-0.4,0.15));
#9971=CARTESIAN_POINT('',(-0.0866025403784439,-0.4,0.15));
#9972=CARTESIAN_POINT('',(-0.173205080756888,-0.4,-2.12115047744981E-17));
#9973=CARTESIAN_POINT('',(-0.0866025403784439,-0.64,0.15));
#9974=CARTESIAN_POINT('',(-0.0866025403784439,-0.4,0.15));
#9975=CARTESIAN_POINT('',(-0.173205080756888,-0.64,-2.12115047744981E-17));
#9976=CARTESIAN_POINT('Origin',(0.0866025403784439,-0.4,0.15));
#9977=CARTESIAN_POINT('',(0.0866025403784439,-0.4,0.15));
#9978=CARTESIAN_POINT('',(-0.0866025403784439,-0.4,0.15));
#9979=CARTESIAN_POINT('',(0.0866025403784439,-0.64,0.15));
#9980=CARTESIAN_POINT('',(0.0866025403784439,-0.4,0.15));
#9981=CARTESIAN_POINT('',(-0.0866025403784439,-0.64,0.15));
#9982=CARTESIAN_POINT('Origin',(0.173205080756888,-0.4,0.));
#9983=CARTESIAN_POINT('',(0.0866025403784439,-0.4,0.15));
#9984=CARTESIAN_POINT('',(0.0866025403784439,-0.64,0.15));
#9985=CARTESIAN_POINT('Origin',(0.,-0.4,-2.77555756156289E-17));
#9986=CARTESIAN_POINT('Origin',(0.,-0.64,-2.77555756156289E-17));
#9987=CARTESIAN_POINT('Origin',(0.,-1.,0.));
#9988=CARTESIAN_POINT('',(-0.1954,-1.,2.39295984553393E-17));
#9989=CARTESIAN_POINT('Origin',(0.,-1.,0.));
#9990=CARTESIAN_POINT('Origin',(0.3,0.4,0.));
#9991=CARTESIAN_POINT('',(-0.3,0.4,-3.67394039744206E-17));
#9992=CARTESIAN_POINT('Origin',(0.,0.4,0.));
#9993=CARTESIAN_POINT('Origin',(0.,0.375,0.));
#9994=CARTESIAN_POINT('',(-0.35,0.35,-4.28626379701573E-17));
#9995=CARTESIAN_POINT('Origin',(0.,0.35,0.));
#9996=CARTESIAN_POINT('',(-0.325,0.375,-3.9801020972289E-17));
#9997=CARTESIAN_POINT('Origin',(0.,0.19,0.));
#9998=CARTESIAN_POINT('',(-0.35,0.03,-4.28626379701574E-17));
#9999=CARTESIAN_POINT('Origin',(0.,0.03,0.));
#10000=CARTESIAN_POINT('',(-0.35,0.19,-4.28626379701574E-17));
#10001=CARTESIAN_POINT('Origin',(0.,0.0149999999999999,0.));
#10002=CARTESIAN_POINT('',(-0.32,-3.29597460435593E-17,-3.91886975727153E-17));
#10003=CARTESIAN_POINT('Origin',(0.,0.,0.));
#10004=CARTESIAN_POINT('',(-0.335,0.0149999999999999,-4.10256677714363E-17));
#10005=CARTESIAN_POINT('Origin',(0.22,0.,0.));
#10006=CARTESIAN_POINT('',(-0.22,-6.93889390390723E-18,-2.69422295812418E-17));
#10007=CARTESIAN_POINT('Origin',(0.,0.,0.));
#10008=CARTESIAN_POINT('Origin',(0.,-0.02,0.));
#10009=CARTESIAN_POINT('',(-0.1954,-0.0492,2.39295984553393E-17));
#10010=CARTESIAN_POINT('Origin',(0.,-0.0492,0.));
#10011=CARTESIAN_POINT('',(-0.21,-0.02,-2.57175827820944E-17));
#10012=CARTESIAN_POINT('Origin',(0.,-0.8,0.));
#10013=CARTESIAN_POINT('',(-0.1954,-0.8,-2.39295984553393E-17));
#10014=CARTESIAN_POINT('',(0.,0.,0.));
#10015=CARTESIAN_POINT('',(0.,0.,0.));
#10016=CARTESIAN_POINT('',(0.,0.,0.));
#10017=CARTESIAN_POINT('',(0.,0.,0.));
#10018=CARTESIAN_POINT('',(0.,0.,0.));
#10019=CARTESIAN_POINT('',(0.,0.,9.6));
#10020=CARTESIAN_POINT('',(0.,0.,0.));
#10021=CARTESIAN_POINT('',(0.,-12.,0.));
#10022=UNCERTAINTY_MEASURE_WITH_UNIT(LENGTH_MEASURE(0.001),#10096,
'DISTANCE_ACCURACY_VALUE',
'Maximum model space distance between geometric entities at asserted c
onnectivities');
#10023=UNCERTAINTY_MEASURE_WITH_UNIT(LENGTH_MEASURE(0.001),#10096,
'DISTANCE_ACCURACY_VALUE',
'Maximum model space distance between geometric entities at asserted c
onnectivities');
#10024=UNCERTAINTY_MEASURE_WITH_UNIT(LENGTH_MEASURE(0.001),#10096,
'DISTANCE_ACCURACY_VALUE',
'Maximum model space distance between geometric entities at asserted c
onnectivities');
#10025=UNCERTAINTY_MEASURE_WITH_UNIT(LENGTH_MEASURE(0.001),#10096,
'DISTANCE_ACCURACY_VALUE',
'Maximum model space distance between geometric entities at asserted c
onnectivities');
#10026=UNCERTAINTY_MEASURE_WITH_UNIT(LENGTH_MEASURE(0.001),#10096,
'DISTANCE_ACCURACY_VALUE',
'Maximum model space distance between geometric entities at asserted c
onnectivities');
#10027=UNCERTAINTY_MEASURE_WITH_UNIT(LENGTH_MEASURE(0.001),#10096,
'DISTANCE_ACCURACY_VALUE',
'Maximum model space distance between geometric entities at asserted c
onnectivities');
#10028=UNCERTAINTY_MEASURE_WITH_UNIT(LENGTH_MEASURE(0.001),#10096,
'DISTANCE_ACCURACY_VALUE',
'Maximum model space distance between geometric entities at asserted c
onnectivities');
#10029=UNCERTAINTY_MEASURE_WITH_UNIT(LENGTH_MEASURE(0.001),#10096,
'DISTANCE_ACCURACY_VALUE',
'Maximum model space distance between geometric entities at asserted c
onnectivities');
#10030=UNCERTAINTY_MEASURE_WITH_UNIT(LENGTH_MEASURE(0.001),#10096,
'DISTANCE_ACCURACY_VALUE',
'Maximum model space distance between geometric entities at asserted c
onnectivities');
#10031=UNCERTAINTY_MEASURE_WITH_UNIT(LENGTH_MEASURE(0.001),#10096,
'DISTANCE_ACCURACY_VALUE',
'Maximum model space distance between geometric entities at asserted c
onnectivities');
#10032=UNCERTAINTY_MEASURE_WITH_UNIT(LENGTH_MEASURE(0.001),#10096,
'DISTANCE_ACCURACY_VALUE',
'Maximum model space distance between geometric entities at asserted c
onnectivities');
#10033=UNCERTAINTY_MEASURE_WITH_UNIT(LENGTH_MEASURE(0.001),#10096,
'DISTANCE_ACCURACY_VALUE',
'Maximum model space distance between geometric entities at asserted c
onnectivities');
#10034=UNCERTAINTY_MEASURE_WITH_UNIT(LENGTH_MEASURE(0.001),#10096,
'DISTANCE_ACCURACY_VALUE',
'Maximum model space distance between geometric entities at asserted c
onnectivities');
#10035=UNCERTAINTY_MEASURE_WITH_UNIT(LENGTH_MEASURE(0.001),#10096,
'DISTANCE_ACCURACY_VALUE',
'Maximum model space distance between geometric entities at asserted c
onnectivities');
#10036=UNCERTAINTY_MEASURE_WITH_UNIT(LENGTH_MEASURE(0.001),#10096,
'DISTANCE_ACCURACY_VALUE',
'Maximum model space distance between geometric entities at asserted c
onnectivities');
#10037=UNCERTAINTY_MEASURE_WITH_UNIT(LENGTH_MEASURE(0.001),#10096,
'DISTANCE_ACCURACY_VALUE',
'Maximum model space distance between geometric entities at asserted c
onnectivities');
#10038=UNCERTAINTY_MEASURE_WITH_UNIT(LENGTH_MEASURE(0.001),#10096,
'DISTANCE_ACCURACY_VALUE',
'Maximum model space distance between geometric entities at asserted c
onnectivities');
#10039=UNCERTAINTY_MEASURE_WITH_UNIT(LENGTH_MEASURE(0.001),#10096,
'DISTANCE_ACCURACY_VALUE',
'Maximum model space distance between geometric entities at asserted c
onnectivities');
#10040=UNCERTAINTY_MEASURE_WITH_UNIT(LENGTH_MEASURE(0.001),#10096,
'DISTANCE_ACCURACY_VALUE',
'Maximum model space distance between geometric entities at asserted c
onnectivities');
#10041=UNCERTAINTY_MEASURE_WITH_UNIT(LENGTH_MEASURE(0.001),#10096,
'DISTANCE_ACCURACY_VALUE',
'Maximum model space distance between geometric entities at asserted c
onnectivities');
#10042=UNCERTAINTY_MEASURE_WITH_UNIT(LENGTH_MEASURE(0.001),#10096,
'DISTANCE_ACCURACY_VALUE',
'Maximum model space distance between geometric entities at asserted c
onnectivities');
#10043=UNCERTAINTY_MEASURE_WITH_UNIT(LENGTH_MEASURE(0.001),#10096,
'DISTANCE_ACCURACY_VALUE',
'Maximum model space distance between geometric entities at asserted c
onnectivities');
#10044=UNCERTAINTY_MEASURE_WITH_UNIT(LENGTH_MEASURE(0.001),#10096,
'DISTANCE_ACCURACY_VALUE',
'Maximum model space distance between geometric entities at asserted c
onnectivities');
#10045=UNCERTAINTY_MEASURE_WITH_UNIT(LENGTH_MEASURE(0.001),#10096,
'DISTANCE_ACCURACY_VALUE',
'Maximum model space distance between geometric entities at asserted c
onnectivities');
#10046=UNCERTAINTY_MEASURE_WITH_UNIT(LENGTH_MEASURE(0.001),#10096,
'DISTANCE_ACCURACY_VALUE',
'Maximum model space distance between geometric entities at asserted c
onnectivities');
#10047=UNCERTAINTY_MEASURE_WITH_UNIT(LENGTH_MEASURE(0.001),#10096,
'DISTANCE_ACCURACY_VALUE',
'Maximum model space distance between geometric entities at asserted c
onnectivities');
#10048=UNCERTAINTY_MEASURE_WITH_UNIT(LENGTH_MEASURE(0.001),#10096,
'DISTANCE_ACCURACY_VALUE',
'Maximum model space distance between geometric entities at asserted c
onnectivities');
#10049=UNCERTAINTY_MEASURE_WITH_UNIT(LENGTH_MEASURE(0.001),#10096,
'DISTANCE_ACCURACY_VALUE',
'Maximum model space distance between geometric entities at asserted c
onnectivities');
#10050=UNCERTAINTY_MEASURE_WITH_UNIT(LENGTH_MEASURE(0.001),#10096,
'DISTANCE_ACCURACY_VALUE',
'Maximum model space distance between geometric entities at asserted c
onnectivities');
#10051=UNCERTAINTY_MEASURE_WITH_UNIT(LENGTH_MEASURE(0.001),#10096,
'DISTANCE_ACCURACY_VALUE',
'Maximum model space distance between geometric entities at asserted c
onnectivities');
#10052=UNCERTAINTY_MEASURE_WITH_UNIT(LENGTH_MEASURE(0.001),#10096,
'DISTANCE_ACCURACY_VALUE',
'Maximum model space distance between geometric entities at asserted c
onnectivities');
#10053=UNCERTAINTY_MEASURE_WITH_UNIT(LENGTH_MEASURE(0.001),#10096,
'DISTANCE_ACCURACY_VALUE',
'Maximum model space distance between geometric entities at asserted c
onnectivities');
#10054=UNCERTAINTY_MEASURE_WITH_UNIT(LENGTH_MEASURE(0.001),#10096,
'DISTANCE_ACCURACY_VALUE',
'Maximum model space distance between geometric entities at asserted c
onnectivities');
#10055=UNCERTAINTY_MEASURE_WITH_UNIT(LENGTH_MEASURE(0.001),#10096,
'DISTANCE_ACCURACY_VALUE',
'Maximum model space distance between geometric entities at asserted c
onnectivities');
#10056=UNCERTAINTY_MEASURE_WITH_UNIT(LENGTH_MEASURE(0.001),#10096,
'DISTANCE_ACCURACY_VALUE',
'Maximum model space distance between geometric entities at asserted c
onnectivities');
#10057=UNCERTAINTY_MEASURE_WITH_UNIT(LENGTH_MEASURE(0.001),#10096,
'DISTANCE_ACCURACY_VALUE',
'Maximum model space distance between geometric entities at asserted c
onnectivities');
#10058=UNCERTAINTY_MEASURE_WITH_UNIT(LENGTH_MEASURE(0.001),#10096,
'DISTANCE_ACCURACY_VALUE',
'Maximum model space distance between geometric entities at asserted c
onnectivities');
#10059=(
GEOMETRIC_REPRESENTATION_CONTEXT(3)
GLOBAL_UNCERTAINTY_ASSIGNED_CONTEXT((#10022))
GLOBAL_UNIT_ASSIGNED_CONTEXT((#10096,#10098,#10099))
REPRESENTATION_CONTEXT('','3D')
);
#10060=(
GEOMETRIC_REPRESENTATION_CONTEXT(3)
GLOBAL_UNCERTAINTY_ASSIGNED_CONTEXT((#10023))
GLOBAL_UNIT_ASSIGNED_CONTEXT((#10096,#10098,#10099))
REPRESENTATION_CONTEXT('','3D')
);
#10061=(
GEOMETRIC_REPRESENTATION_CONTEXT(3)
GLOBAL_UNCERTAINTY_ASSIGNED_CONTEXT((#10024))
GLOBAL_UNIT_ASSIGNED_CONTEXT((#10096,#10098,#10099))
REPRESENTATION_CONTEXT('','3D')
);
#10062=(
GEOMETRIC_REPRESENTATION_CONTEXT(3)
GLOBAL_UNCERTAINTY_ASSIGNED_CONTEXT((#10025))
GLOBAL_UNIT_ASSIGNED_CONTEXT((#10096,#10098,#10099))
REPRESENTATION_CONTEXT('','3D')
);
#10063=(
GEOMETRIC_REPRESENTATION_CONTEXT(3)
GLOBAL_UNCERTAINTY_ASSIGNED_CONTEXT((#10026))
GLOBAL_UNIT_ASSIGNED_CONTEXT((#10096,#10098,#10099))
REPRESENTATION_CONTEXT('','3D')
);
#10064=(
GEOMETRIC_REPRESENTATION_CONTEXT(3)
GLOBAL_UNCERTAINTY_ASSIGNED_CONTEXT((#10027))
GLOBAL_UNIT_ASSIGNED_CONTEXT((#10096,#10098,#10099))
REPRESENTATION_CONTEXT('','3D')
);
#10065=(
GEOMETRIC_REPRESENTATION_CONTEXT(3)
GLOBAL_UNCERTAINTY_ASSIGNED_CONTEXT((#10028))
GLOBAL_UNIT_ASSIGNED_CONTEXT((#10096,#10098,#10099))
REPRESENTATION_CONTEXT('','3D')
);
#10066=(
GEOMETRIC_REPRESENTATION_CONTEXT(3)
GLOBAL_UNCERTAINTY_ASSIGNED_CONTEXT((#10029))
GLOBAL_UNIT_ASSIGNED_CONTEXT((#10096,#10098,#10099))
REPRESENTATION_CONTEXT('','3D')
);
#10067=(
GEOMETRIC_REPRESENTATION_CONTEXT(3)
GLOBAL_UNCERTAINTY_ASSIGNED_CONTEXT((#10030))
GLOBAL_UNIT_ASSIGNED_CONTEXT((#10096,#10098,#10099))
REPRESENTATION_CONTEXT('','3D')
);
#10068=(
GEOMETRIC_REPRESENTATION_CONTEXT(3)
GLOBAL_UNCERTAINTY_ASSIGNED_CONTEXT((#10031))
GLOBAL_UNIT_ASSIGNED_CONTEXT((#10096,#10098,#10099))
REPRESENTATION_CONTEXT('','3D')
);
#10069=(
GEOMETRIC_REPRESENTATION_CONTEXT(3)
GLOBAL_UNCERTAINTY_ASSIGNED_CONTEXT((#10032))
GLOBAL_UNIT_ASSIGNED_CONTEXT((#10096,#10098,#10099))
REPRESENTATION_CONTEXT('','3D')
);
#10070=(
GEOMETRIC_REPRESENTATION_CONTEXT(3)
GLOBAL_UNCERTAINTY_ASSIGNED_CONTEXT((#10033))
GLOBAL_UNIT_ASSIGNED_CONTEXT((#10096,#10098,#10099))
REPRESENTATION_CONTEXT('','3D')
);
#10071=(
GEOMETRIC_REPRESENTATION_CONTEXT(3)
GLOBAL_UNCERTAINTY_ASSIGNED_CONTEXT((#10034))
GLOBAL_UNIT_ASSIGNED_CONTEXT((#10096,#10098,#10099))
REPRESENTATION_CONTEXT('','3D')
);
#10072=(
GEOMETRIC_REPRESENTATION_CONTEXT(3)
GLOBAL_UNCERTAINTY_ASSIGNED_CONTEXT((#10035))
GLOBAL_UNIT_ASSIGNED_CONTEXT((#10096,#10098,#10099))
REPRESENTATION_CONTEXT('','3D')
);
#10073=(
GEOMETRIC_REPRESENTATION_CONTEXT(3)
GLOBAL_UNCERTAINTY_ASSIGNED_CONTEXT((#10036))
GLOBAL_UNIT_ASSIGNED_CONTEXT((#10096,#10098,#10099))
REPRESENTATION_CONTEXT('','3D')
);
#10074=(
GEOMETRIC_REPRESENTATION_CONTEXT(3)
GLOBAL_UNCERTAINTY_ASSIGNED_CONTEXT((#10037))
GLOBAL_UNIT_ASSIGNED_CONTEXT((#10096,#10098,#10099))
REPRESENTATION_CONTEXT('','3D')
);
#10075=(
GEOMETRIC_REPRESENTATION_CONTEXT(3)
GLOBAL_UNCERTAINTY_ASSIGNED_CONTEXT((#10038))
GLOBAL_UNIT_ASSIGNED_CONTEXT((#10096,#10098,#10099))
REPRESENTATION_CONTEXT('','3D')
);
#10076=(
GEOMETRIC_REPRESENTATION_CONTEXT(3)
GLOBAL_UNCERTAINTY_ASSIGNED_CONTEXT((#10039))
GLOBAL_UNIT_ASSIGNED_CONTEXT((#10096,#10098,#10099))
REPRESENTATION_CONTEXT('','3D')
);
#10077=(
GEOMETRIC_REPRESENTATION_CONTEXT(3)
GLOBAL_UNCERTAINTY_ASSIGNED_CONTEXT((#10040))
GLOBAL_UNIT_ASSIGNED_CONTEXT((#10096,#10098,#10099))
REPRESENTATION_CONTEXT('','3D')
);
#10078=(
GEOMETRIC_REPRESENTATION_CONTEXT(3)
GLOBAL_UNCERTAINTY_ASSIGNED_CONTEXT((#10041))
GLOBAL_UNIT_ASSIGNED_CONTEXT((#10096,#10098,#10099))
REPRESENTATION_CONTEXT('','3D')
);
#10079=(
GEOMETRIC_REPRESENTATION_CONTEXT(3)
GLOBAL_UNCERTAINTY_ASSIGNED_CONTEXT((#10042))
GLOBAL_UNIT_ASSIGNED_CONTEXT((#10096,#10098,#10099))
REPRESENTATION_CONTEXT('','3D')
);
#10080=(
GEOMETRIC_REPRESENTATION_CONTEXT(3)
GLOBAL_UNCERTAINTY_ASSIGNED_CONTEXT((#10043))
GLOBAL_UNIT_ASSIGNED_CONTEXT((#10096,#10098,#10099))
REPRESENTATION_CONTEXT('','3D')
);
#10081=(
GEOMETRIC_REPRESENTATION_CONTEXT(3)
GLOBAL_UNCERTAINTY_ASSIGNED_CONTEXT((#10044))
GLOBAL_UNIT_ASSIGNED_CONTEXT((#10096,#10098,#10099))
REPRESENTATION_CONTEXT('','3D')
);
#10082=(
GEOMETRIC_REPRESENTATION_CONTEXT(3)
GLOBAL_UNCERTAINTY_ASSIGNED_CONTEXT((#10045))
GLOBAL_UNIT_ASSIGNED_CONTEXT((#10096,#10098,#10099))
REPRESENTATION_CONTEXT('','3D')
);
#10083=(
GEOMETRIC_REPRESENTATION_CONTEXT(3)
GLOBAL_UNCERTAINTY_ASSIGNED_CONTEXT((#10046))
GLOBAL_UNIT_ASSIGNED_CONTEXT((#10096,#10098,#10099))
REPRESENTATION_CONTEXT('','3D')
);
#10084=(
GEOMETRIC_REPRESENTATION_CONTEXT(3)
GLOBAL_UNCERTAINTY_ASSIGNED_CONTEXT((#10047))
GLOBAL_UNIT_ASSIGNED_CONTEXT((#10096,#10098,#10099))
REPRESENTATION_CONTEXT('','3D')
);
#10085=(
GEOMETRIC_REPRESENTATION_CONTEXT(3)
GLOBAL_UNCERTAINTY_ASSIGNED_CONTEXT((#10048))
GLOBAL_UNIT_ASSIGNED_CONTEXT((#10096,#10098,#10099))
REPRESENTATION_CONTEXT('','3D')
);
#10086=(
GEOMETRIC_REPRESENTATION_CONTEXT(3)
GLOBAL_UNCERTAINTY_ASSIGNED_CONTEXT((#10049))
GLOBAL_UNIT_ASSIGNED_CONTEXT((#10096,#10098,#10099))
REPRESENTATION_CONTEXT('','3D')
);
#10087=(
GEOMETRIC_REPRESENTATION_CONTEXT(3)
GLOBAL_UNCERTAINTY_ASSIGNED_CONTEXT((#10050))
GLOBAL_UNIT_ASSIGNED_CONTEXT((#10096,#10098,#10099))
REPRESENTATION_CONTEXT('','3D')
);
#10088=(
GEOMETRIC_REPRESENTATION_CONTEXT(3)
GLOBAL_UNCERTAINTY_ASSIGNED_CONTEXT((#10051))
GLOBAL_UNIT_ASSIGNED_CONTEXT((#10096,#10098,#10099))
REPRESENTATION_CONTEXT('','3D')
);
#10089=(
GEOMETRIC_REPRESENTATION_CONTEXT(3)
GLOBAL_UNCERTAINTY_ASSIGNED_CONTEXT((#10052))
GLOBAL_UNIT_ASSIGNED_CONTEXT((#10096,#10098,#10099))
REPRESENTATION_CONTEXT('','3D')
);
#10090=(
GEOMETRIC_REPRESENTATION_CONTEXT(3)
GLOBAL_UNCERTAINTY_ASSIGNED_CONTEXT((#10053))
GLOBAL_UNIT_ASSIGNED_CONTEXT((#10096,#10098,#10099))
REPRESENTATION_CONTEXT('','3D')
);
#10091=(
GEOMETRIC_REPRESENTATION_CONTEXT(3)
GLOBAL_UNCERTAINTY_ASSIGNED_CONTEXT((#10054))
GLOBAL_UNIT_ASSIGNED_CONTEXT((#10096,#10098,#10099))
REPRESENTATION_CONTEXT('','3D')
);
#10092=(
GEOMETRIC_REPRESENTATION_CONTEXT(3)
GLOBAL_UNCERTAINTY_ASSIGNED_CONTEXT((#10055))
GLOBAL_UNIT_ASSIGNED_CONTEXT((#10096,#10098,#10099))
REPRESENTATION_CONTEXT('','3D')
);
#10093=(
GEOMETRIC_REPRESENTATION_CONTEXT(3)
GLOBAL_UNCERTAINTY_ASSIGNED_CONTEXT((#10056))
GLOBAL_UNIT_ASSIGNED_CONTEXT((#10096,#10098,#10099))
REPRESENTATION_CONTEXT('','3D')
);
#10094=(
GEOMETRIC_REPRESENTATION_CONTEXT(3)
GLOBAL_UNCERTAINTY_ASSIGNED_CONTEXT((#10057))
GLOBAL_UNIT_ASSIGNED_CONTEXT((#10096,#10098,#10099))
REPRESENTATION_CONTEXT('','3D')
);
#10095=(
GEOMETRIC_REPRESENTATION_CONTEXT(3)
GLOBAL_UNCERTAINTY_ASSIGNED_CONTEXT((#10058))
GLOBAL_UNIT_ASSIGNED_CONTEXT((#10096,#10098,#10099))
REPRESENTATION_CONTEXT('','3D')
);
#10096=(
LENGTH_UNIT()
NAMED_UNIT(*)
SI_UNIT(.CENTI.,.METRE.)
);
#10097=(
LENGTH_UNIT()
NAMED_UNIT(*)
SI_UNIT($,.METRE.)
);
#10098=(
NAMED_UNIT(*)
PLANE_ANGLE_UNIT()
SI_UNIT($,.RADIAN.)
);
#10099=(
NAMED_UNIT(*)
SI_UNIT($,.STERADIAN.)
SOLID_ANGLE_UNIT()
);
#10100=SHAPE_DEFINITION_REPRESENTATION(#10136,#10247);
#10101=SHAPE_DEFINITION_REPRESENTATION(#10137,#10248);
#10102=SHAPE_DEFINITION_REPRESENTATION(#10138,#10249);
#10103=SHAPE_DEFINITION_REPRESENTATION(#10139,#10250);
#10104=SHAPE_DEFINITION_REPRESENTATION(#10140,#10251);
#10105=SHAPE_DEFINITION_REPRESENTATION(#10141,#10252);
#10106=SHAPE_DEFINITION_REPRESENTATION(#10142,#10253);
#10107=SHAPE_DEFINITION_REPRESENTATION(#10143,#10254);
#10108=SHAPE_DEFINITION_REPRESENTATION(#10144,#10255);
#10109=SHAPE_DEFINITION_REPRESENTATION(#10145,#10256);
#10110=SHAPE_DEFINITION_REPRESENTATION(#10146,#10257);
#10111=SHAPE_DEFINITION_REPRESENTATION(#10147,#10258);
#10112=SHAPE_DEFINITION_REPRESENTATION(#10148,#10259);
#10113=SHAPE_DEFINITION_REPRESENTATION(#10149,#10260);
#10114=SHAPE_DEFINITION_REPRESENTATION(#10150,#10261);
#10115=SHAPE_DEFINITION_REPRESENTATION(#10151,#10262);
#10116=SHAPE_DEFINITION_REPRESENTATION(#10152,#10263);
#10117=SHAPE_DEFINITION_REPRESENTATION(#10188,#10264);
#10118=SHAPE_DEFINITION_REPRESENTATION(#10189,#10265);
#10119=SHAPE_DEFINITION_REPRESENTATION(#10190,#10266);
#10120=SHAPE_DEFINITION_REPRESENTATION(#10191,#10267);
#10121=SHAPE_DEFINITION_REPRESENTATION(#10192,#10268);
#10122=SHAPE_DEFINITION_REPRESENTATION(#10193,#10269);
#10123=SHAPE_DEFINITION_REPRESENTATION(#10194,#10270);
#10124=SHAPE_DEFINITION_REPRESENTATION(#10195,#10271);
#10125=SHAPE_DEFINITION_REPRESENTATION(#10196,#10272);
#10126=SHAPE_DEFINITION_REPRESENTATION(#10197,#10273);
#10127=SHAPE_DEFINITION_REPRESENTATION(#10198,#10274);
#10128=SHAPE_DEFINITION_REPRESENTATION(#10199,#10275);
#10129=SHAPE_DEFINITION_REPRESENTATION(#10232,#10276);
#10130=SHAPE_DEFINITION_REPRESENTATION(#10233,#10277);
#10131=SHAPE_DEFINITION_REPRESENTATION(#10234,#10278);
#10132=SHAPE_DEFINITION_REPRESENTATION(#10235,#10279);
#10133=SHAPE_DEFINITION_REPRESENTATION(#10236,#10280);
#10134=SHAPE_DEFINITION_REPRESENTATION(#10237,#10281);
#10135=SHAPE_DEFINITION_REPRESENTATION(#10238,#10282);
#10136=PRODUCT_DEFINITION_SHAPE('',$,#10284);
#10137=PRODUCT_DEFINITION_SHAPE('',$,#10285);
#10138=PRODUCT_DEFINITION_SHAPE('',$,#10286);
#10139=PRODUCT_DEFINITION_SHAPE('',$,#10287);
#10140=PRODUCT_DEFINITION_SHAPE('',$,#10288);
#10141=PRODUCT_DEFINITION_SHAPE('',$,#10289);
#10142=PRODUCT_DEFINITION_SHAPE('',$,#10290);
#10143=PRODUCT_DEFINITION_SHAPE('',$,#10291);
#10144=PRODUCT_DEFINITION_SHAPE('',$,#10292);
#10145=PRODUCT_DEFINITION_SHAPE('',$,#10293);
#10146=PRODUCT_DEFINITION_SHAPE('',$,#10294);
#10147=PRODUCT_DEFINITION_SHAPE('',$,#10295);
#10148=PRODUCT_DEFINITION_SHAPE('',$,#10296);
#10149=PRODUCT_DEFINITION_SHAPE('',$,#10297);
#10150=PRODUCT_DEFINITION_SHAPE('',$,#10298);
#10151=PRODUCT_DEFINITION_SHAPE('',$,#10299);
#10152=PRODUCT_DEFINITION_SHAPE('',$,#10300);
#10153=PRODUCT_DEFINITION_SHAPE($,$,#252);
#10154=PRODUCT_DEFINITION_SHAPE($,$,#253);
#10155=PRODUCT_DEFINITION_SHAPE($,$,#254);
#10156=PRODUCT_DEFINITION_SHAPE($,$,#255);
#10157=PRODUCT_DEFINITION_SHAPE($,$,#256);
#10158=PRODUCT_DEFINITION_SHAPE($,$,#257);
#10159=PRODUCT_DEFINITION_SHAPE($,$,#258);
#10160=PRODUCT_DEFINITION_SHAPE($,$,#259);
#10161=PRODUCT_DEFINITION_SHAPE($,$,#260);
#10162=PRODUCT_DEFINITION_SHAPE($,$,#261);
#10163=PRODUCT_DEFINITION_SHAPE($,$,#262);
#10164=PRODUCT_DEFINITION_SHAPE($,$,#263);
#10165=PRODUCT_DEFINITION_SHAPE($,$,#264);
#10166=PRODUCT_DEFINITION_SHAPE($,$,#265);
#10167=PRODUCT_DEFINITION_SHAPE($,$,#266);
#10168=PRODUCT_DEFINITION_SHAPE($,$,#267);
#10169=PRODUCT_DEFINITION_SHAPE($,$,#268);
#10170=PRODUCT_DEFINITION_SHAPE($,$,#269);
#10171=PRODUCT_DEFINITION_SHAPE($,$,#270);
#10172=PRODUCT_DEFINITION_SHAPE($,$,#271);
#10173=PRODUCT_DEFINITION_SHAPE($,$,#272);
#10174=PRODUCT_DEFINITION_SHAPE($,$,#273);
#10175=PRODUCT_DEFINITION_SHAPE($,$,#274);
#10176=PRODUCT_DEFINITION_SHAPE($,$,#275);
#10177=PRODUCT_DEFINITION_SHAPE($,$,#276);
#10178=PRODUCT_DEFINITION_SHAPE($,$,#277);
#10179=PRODUCT_DEFINITION_SHAPE($,$,#278);
#10180=PRODUCT_DEFINITION_SHAPE($,$,#279);
#10181=PRODUCT_DEFINITION_SHAPE($,$,#280);
#10182=PRODUCT_DEFINITION_SHAPE($,$,#281);
#10183=PRODUCT_DEFINITION_SHAPE($,$,#282);
#10184=PRODUCT_DEFINITION_SHAPE($,$,#283);
#10185=PRODUCT_DEFINITION_SHAPE($,$,#284);
#10186=PRODUCT_DEFINITION_SHAPE($,$,#285);
#10187=PRODUCT_DEFINITION_SHAPE($,$,#286);
#10188=PRODUCT_DEFINITION_SHAPE('',$,#10301);
#10189=PRODUCT_DEFINITION_SHAPE('',$,#10302);
#10190=PRODUCT_DEFINITION_SHAPE('',$,#10303);
#10191=PRODUCT_DEFINITION_SHAPE('',$,#10304);
#10192=PRODUCT_DEFINITION_SHAPE('',$,#10305);
#10193=PRODUCT_DEFINITION_SHAPE('',$,#10306);
#10194=PRODUCT_DEFINITION_SHAPE('',$,#10307);
#10195=PRODUCT_DEFINITION_SHAPE('',$,#10308);
#10196=PRODUCT_DEFINITION_SHAPE('',$,#10309);
#10197=PRODUCT_DEFINITION_SHAPE('',$,#10310);
#10198=PRODUCT_DEFINITION_SHAPE('',$,#10311);
#10199=PRODUCT_DEFINITION_SHAPE('',$,#10312);
#10200=PRODUCT_DEFINITION_SHAPE($,$,#287);
#10201=PRODUCT_DEFINITION_SHAPE($,$,#288);
#10202=PRODUCT_DEFINITION_SHAPE($,$,#289);
#10203=PRODUCT_DEFINITION_SHAPE($,$,#290);
#10204=PRODUCT_DEFINITION_SHAPE($,$,#291);
#10205=PRODUCT_DEFINITION_SHAPE($,$,#292);
#10206=PRODUCT_DEFINITION_SHAPE($,$,#293);
#10207=PRODUCT_DEFINITION_SHAPE($,$,#294);
#10208=PRODUCT_DEFINITION_SHAPE($,$,#295);
#10209=PRODUCT_DEFINITION_SHAPE($,$,#296);
#10210=PRODUCT_DEFINITION_SHAPE($,$,#297);
#10211=PRODUCT_DEFINITION_SHAPE($,$,#298);
#10212=PRODUCT_DEFINITION_SHAPE($,$,#299);
#10213=PRODUCT_DEFINITION_SHAPE($,$,#300);
#10214=PRODUCT_DEFINITION_SHAPE($,$,#301);
#10215=PRODUCT_DEFINITION_SHAPE($,$,#302);
#10216=PRODUCT_DEFINITION_SHAPE($,$,#303);
#10217=PRODUCT_DEFINITION_SHAPE($,$,#304);
#10218=PRODUCT_DEFINITION_SHAPE($,$,#305);
#10219=PRODUCT_DEFINITION_SHAPE($,$,#306);
#10220=PRODUCT_DEFINITION_SHAPE($,$,#307);
#10221=PRODUCT_DEFINITION_SHAPE($,$,#308);
#10222=PRODUCT_DEFINITION_SHAPE($,$,#309);
#10223=PRODUCT_DEFINITION_SHAPE($,$,#310);
#10224=PRODUCT_DEFINITION_SHAPE($,$,#311);
#10225=PRODUCT_DEFINITION_SHAPE($,$,#312);
#10226=PRODUCT_DEFINITION_SHAPE($,$,#313);
#10227=PRODUCT_DEFINITION_SHAPE($,$,#314);
#10228=PRODUCT_DEFINITION_SHAPE($,$,#315);
#10229=PRODUCT_DEFINITION_SHAPE($,$,#316);
#10230=PRODUCT_DEFINITION_SHAPE($,$,#317);
#10231=PRODUCT_DEFINITION_SHAPE($,$,#318);
#10232=PRODUCT_DEFINITION_SHAPE('',$,#10313);
#10233=PRODUCT_DEFINITION_SHAPE('',$,#10314);
#10234=PRODUCT_DEFINITION_SHAPE('',$,#10315);
#10235=PRODUCT_DEFINITION_SHAPE('',$,#10316);
#10236=PRODUCT_DEFINITION_SHAPE('',$,#10317);
#10237=PRODUCT_DEFINITION_SHAPE('',$,#10318);
#10238=PRODUCT_DEFINITION_SHAPE('',$,#10319);
#10239=PRODUCT_DEFINITION_SHAPE($,$,#319);
#10240=PRODUCT_DEFINITION_SHAPE($,$,#320);
#10241=PRODUCT_DEFINITION_SHAPE($,$,#321);
#10242=PRODUCT_DEFINITION_SHAPE($,$,#322);
#10243=PRODUCT_DEFINITION_SHAPE($,$,#323);
#10244=PRODUCT_DEFINITION_SHAPE($,$,#324);
#10245=PRODUCT_DEFINITION_SHAPE($,$,#325);
#10246=PRODUCT_DEFINITION_SHAPE($,$,#326);
#10247=SHAPE_REPRESENTATION('',(#5905,#6617,#6618),#10059);
#10248=SHAPE_REPRESENTATION('',(#5906,#6476,#6477,#6478,#6479,#6480,#6481,
#6482,#6483,#6484,#6485,#6486,#6487,#6488,#6489,#6490,#6491,#6492,#6493,
#6494,#6495,#6496,#6497,#6498,#6499,#6500,#6501,#6502,#6503,#6504,#6505,
#6506,#6507),#10060);
#10249=SHAPE_REPRESENTATION('',(#5907,#6188,#6189,#6190,#6191,#6192,#6193,
#6194,#6195,#6196,#6197,#6198,#6199,#6200,#6201,#6202,#6203,#6204,#6205,
#6206,#6207,#6208,#6209,#6210,#6211,#6212,#6213,#6214,#6215,#6216,#6217,
#6218,#6219,#6220,#6221,#6222),#10061);
#10250=SHAPE_REPRESENTATION('',(#5908),#10062);
#10251=SHAPE_REPRESENTATION('',(#5951),#10063);
#10252=SHAPE_REPRESENTATION('',(#5994),#10064);
#10253=SHAPE_REPRESENTATION('',(#6021),#10065);
#10254=SHAPE_REPRESENTATION('',(#6034),#10066);
#10255=SHAPE_REPRESENTATION('',(#6038),#10067);
#10256=SHAPE_REPRESENTATION('',(#6051),#10068);
#10257=SHAPE_REPRESENTATION('',(#6081),#10069);
#10258=SHAPE_REPRESENTATION('',(#6092),#10070);
#10259=SHAPE_REPRESENTATION('',(#6120),#10071);
#10260=SHAPE_REPRESENTATION('',(#6131),#10072);
#10261=SHAPE_REPRESENTATION('',(#6147),#10073);
#10262=SHAPE_REPRESENTATION('',(#6156),#10074);
#10263=SHAPE_REPRESENTATION('',(#6182),#10075);
#10264=SHAPE_REPRESENTATION('',(#6223),#10076);
#10265=SHAPE_REPRESENTATION('',(#6232),#10077);
#10266=SHAPE_REPRESENTATION('',(#6284),#10078);
#10267=SHAPE_REPRESENTATION('',(#6293),#10079);
#10268=SHAPE_REPRESENTATION('',(#6302),#10080);
#10269=SHAPE_REPRESENTATION('',(#6311),#10081);
#10270=SHAPE_REPRESENTATION('',(#6351),#10082);
#10271=SHAPE_REPRESENTATION('',(#6375),#10083);
#10272=SHAPE_REPRESENTATION('',(#6400),#10084);
#10273=SHAPE_REPRESENTATION('',(#6425),#10085);
#10274=SHAPE_REPRESENTATION('',(#6451),#10086);
#10275=SHAPE_REPRESENTATION('',(#6460),#10087);
#10276=SHAPE_REPRESENTATION('',(#6508,#6611,#6612,#6613,#6614,#6615,#6616),
#10088);
#10277=SHAPE_REPRESENTATION('',(#6509),#10089);
#10278=SHAPE_REPRESENTATION('',(#6525),#10090);
#10279=SHAPE_REPRESENTATION('',(#6560),#10091);
#10280=SHAPE_REPRESENTATION('',(#6571),#10092);
#10281=SHAPE_REPRESENTATION('',(#6580),#10093);
#10282=SHAPE_REPRESENTATION('',(#6587),#10094);
#10283=PRODUCT_DEFINITION_CONTEXT('part definition',#10393,'design');
#10284=PRODUCT_DEFINITION('PAT-115','PAT-115',#10320,#10283);
#10285=PRODUCT_DEFINITION('Pipe loop union and valve body',
'Pipe loop union and valve body',#10321,#10283);
#10286=PRODUCT_DEFINITION('Bypass valve body','Bypass valve body',#10322,
#10283);
#10287=PRODUCT_DEFINITION('Body inlet half','Body inlet half',#10323,#10283);
#10288=PRODUCT_DEFINITION('Body outlet half','Body outlet half',#10324,
#10283);
#10289=PRODUCT_DEFINITION('Split-body gasket','Split-body gasket',#10325,
#10283);
#10290=PRODUCT_DEFINITION('Stem guide','Stem guide',#10326,#10283);
#10291=PRODUCT_DEFINITION('Packing ring','Packing ring',#10327,#10283);
#10292=PRODUCT_DEFINITION('Packing retainer','Packing retainer',#10328,
#10283);
#10293=PRODUCT_DEFINITION('Lever stop bridge','Lever stop bridge',#10329,
#10283);
#10294=PRODUCT_DEFINITION('Ball seat','Ball seat',#10330,#10283);
#10295=PRODUCT_DEFINITION('M5x70 body screw','M5x70 body screw',#10331,
#10283);
#10296=PRODUCT_DEFINITION('Flat Washer - M5','Flat Washer - M5',#10332,
#10283);
#10297=PRODUCT_DEFINITION('Hex Nut - M5','Hex Nut - M5',#10333,#10283);
#10298=PRODUCT_DEFINITION('Bridge spacer','Bridge spacer',#10334,#10283);
#10299=PRODUCT_DEFINITION('Cap Screw - M4x16','Cap Screw - M4x16',#10335,
#10283);
#10300=PRODUCT_DEFINITION('Stop pin','Stop pin',#10336,#10283);
#10301=PRODUCT_DEFINITION('Union gasket','Union gasket',#10337,#10283);
#10302=PRODUCT_DEFINITION('Bypass tee','Bypass tee',#10338,#10283);
#10303=PRODUCT_DEFINITION('Main-run pipe','Main-run pipe',#10339,#10283);
#10304=PRODUCT_DEFINITION('Bypass side pipe','Bypass side pipe',#10340,
#10283);
#10305=PRODUCT_DEFINITION('Bypass valve pipe','Bypass valve pipe',#10341,
#10283);
#10306=PRODUCT_DEFINITION(
'Pipe Elbow - 90 Degrees, 1-2 Inch Tapered Pipe Thread',
'Pipe Elbow - 90 Degrees, 1-2 Inch Tapered Pipe Thread',#10342,#10283);
#10307=PRODUCT_DEFINITION(
'Hex Pipe Nipple - 1-2 Inch Tapered Pipe Thread',
'Hex Pipe Nipple - 1-2 Inch Tapered Pipe Thread',#10343,#10283);
#10308=PRODUCT_DEFINITION('Union half A','Union half A',#10344,#10283);
#10309=PRODUCT_DEFINITION('Union half B','Union half B',#10345,#10283);
#10310=PRODUCT_DEFINITION('Cap Screw - M8x30','Cap Screw - M8x30',#10346,
#10283);
#10311=PRODUCT_DEFINITION('Flat Washer - M8','Flat Washer - M8',#10347,
#10283);
#10312=PRODUCT_DEFINITION('Hex Nut - M8','Hex Nut - M8',#10348,#10283);
#10313=PRODUCT_DEFINITION('Bypass valve rotor','Bypass valve rotor',#10349,
#10283);
#10314=PRODUCT_DEFINITION('Ported ball','Ported ball',#10350,#10283);
#10315=PRODUCT_DEFINITION('Stem','Stem',#10351,#10283);
#10316=PRODUCT_DEFINITION('Lever','Lever',#10352,#10283);
#10317=PRODUCT_DEFINITION('Lever keeper','Lever keeper',#10353,#10283);
#10318=PRODUCT_DEFINITION('Bonded grip','Bonded grip',#10354,#10283);
#10319=PRODUCT_DEFINITION('M4x10 Cap Screw','M4x10 Cap Screw',#10355,#10283);
#10320=PRODUCT_DEFINITION_FORMATION('',$,#10395);
#10321=PRODUCT_DEFINITION_FORMATION('',$,#10396);
#10322=PRODUCT_DEFINITION_FORMATION('',$,#10397);
#10323=PRODUCT_DEFINITION_FORMATION('',$,#10398);
#10324=PRODUCT_DEFINITION_FORMATION('',$,#10399);
#10325=PRODUCT_DEFINITION_FORMATION('',$,#10400);
#10326=PRODUCT_DEFINITION_FORMATION('',$,#10401);
#10327=PRODUCT_DEFINITION_FORMATION('',$,#10402);
#10328=PRODUCT_DEFINITION_FORMATION('',$,#10403);
#10329=PRODUCT_DEFINITION_FORMATION('',$,#10404);
#10330=PRODUCT_DEFINITION_FORMATION('',$,#10405);
#10331=PRODUCT_DEFINITION_FORMATION('',$,#10406);
#10332=PRODUCT_DEFINITION_FORMATION('',$,#10407);
#10333=PRODUCT_DEFINITION_FORMATION('',$,#10408);
#10334=PRODUCT_DEFINITION_FORMATION('',$,#10409);
#10335=PRODUCT_DEFINITION_FORMATION('',$,#10410);
#10336=PRODUCT_DEFINITION_FORMATION('',$,#10411);
#10337=PRODUCT_DEFINITION_FORMATION('',$,#10412);
#10338=PRODUCT_DEFINITION_FORMATION('',$,#10413);
#10339=PRODUCT_DEFINITION_FORMATION('',$,#10414);
#10340=PRODUCT_DEFINITION_FORMATION('',$,#10415);
#10341=PRODUCT_DEFINITION_FORMATION('',$,#10416);
#10342=PRODUCT_DEFINITION_FORMATION('',$,#10417);
#10343=PRODUCT_DEFINITION_FORMATION('',$,#10418);
#10344=PRODUCT_DEFINITION_FORMATION('',$,#10419);
#10345=PRODUCT_DEFINITION_FORMATION('',$,#10420);
#10346=PRODUCT_DEFINITION_FORMATION('',$,#10421);
#10347=PRODUCT_DEFINITION_FORMATION('',$,#10422);
#10348=PRODUCT_DEFINITION_FORMATION('',$,#10423);
#10349=PRODUCT_DEFINITION_FORMATION('',$,#10424);
#10350=PRODUCT_DEFINITION_FORMATION('',$,#10425);
#10351=PRODUCT_DEFINITION_FORMATION('',$,#10426);
#10352=PRODUCT_DEFINITION_FORMATION('',$,#10427);
#10353=PRODUCT_DEFINITION_FORMATION('',$,#10428);
#10354=PRODUCT_DEFINITION_FORMATION('',$,#10429);
#10355=PRODUCT_DEFINITION_FORMATION('',$,#10430);
#10356=PRODUCT_RELATED_PRODUCT_CATEGORY('PAT-115','PAT-115',(#10395));
#10357=PRODUCT_RELATED_PRODUCT_CATEGORY(
'Pipe loop union and valve body','Pipe loop union and valve body',(#10396));
#10358=PRODUCT_RELATED_PRODUCT_CATEGORY('Bypass valve body',
'Bypass valve body',(#10397));
#10359=PRODUCT_RELATED_PRODUCT_CATEGORY('Body inlet half',
'Body inlet half',(#10398));
#10360=PRODUCT_RELATED_PRODUCT_CATEGORY('Body outlet half',
'Body outlet half',(#10399));
#10361=PRODUCT_RELATED_PRODUCT_CATEGORY('Split-body gasket',
'Split-body gasket',(#10400));
#10362=PRODUCT_RELATED_PRODUCT_CATEGORY('Stem guide','Stem guide',(#10401));
#10363=PRODUCT_RELATED_PRODUCT_CATEGORY('Packing ring','Packing ring',(#10402));
#10364=PRODUCT_RELATED_PRODUCT_CATEGORY('Packing retainer',
'Packing retainer',(#10403));
#10365=PRODUCT_RELATED_PRODUCT_CATEGORY('Lever stop bridge',
'Lever stop bridge',(#10404));
#10366=PRODUCT_RELATED_PRODUCT_CATEGORY('Ball seat','Ball seat',(#10405));
#10367=PRODUCT_RELATED_PRODUCT_CATEGORY('M5x70 body screw',
'M5x70 body screw',(#10406));
#10368=PRODUCT_RELATED_PRODUCT_CATEGORY('Flat Washer - M5',
'Flat Washer - M5',(#10407));
#10369=PRODUCT_RELATED_PRODUCT_CATEGORY('Hex Nut - M5','Hex Nut - M5',(#10408));
#10370=PRODUCT_RELATED_PRODUCT_CATEGORY('Bridge spacer','Bridge spacer',
(#10409));
#10371=PRODUCT_RELATED_PRODUCT_CATEGORY('Cap Screw - M4x16',
'Cap Screw - M4x16',(#10410));
#10372=PRODUCT_RELATED_PRODUCT_CATEGORY('Stop pin','Stop pin',(#10411));
#10373=PRODUCT_RELATED_PRODUCT_CATEGORY('Union gasket','Union gasket',(#10412));
#10374=PRODUCT_RELATED_PRODUCT_CATEGORY('Bypass tee','Bypass tee',(#10413));
#10375=PRODUCT_RELATED_PRODUCT_CATEGORY('Main-run pipe','Main-run pipe',
(#10414));
#10376=PRODUCT_RELATED_PRODUCT_CATEGORY('Bypass side pipe',
'Bypass side pipe',(#10415));
#10377=PRODUCT_RELATED_PRODUCT_CATEGORY('Bypass valve pipe',
'Bypass valve pipe',(#10416));
#10378=PRODUCT_RELATED_PRODUCT_CATEGORY(
'Pipe Elbow - 90 Degrees, 1-2 Inch Tapered Pipe Thread',
'Pipe Elbow - 90 Degrees, 1-2 Inch Tapered Pipe Thread',(#10417));
#10379=PRODUCT_RELATED_PRODUCT_CATEGORY(
'Hex Pipe Nipple - 1-2 Inch Tapered Pipe Thread',
'Hex Pipe Nipple - 1-2 Inch Tapered Pipe Thread',(#10418));
#10380=PRODUCT_RELATED_PRODUCT_CATEGORY('Union half A','Union half A',(#10419));
#10381=PRODUCT_RELATED_PRODUCT_CATEGORY('Union half B','Union half B',(#10420));
#10382=PRODUCT_RELATED_PRODUCT_CATEGORY('Cap Screw - M8x30',
'Cap Screw - M8x30',(#10421));
#10383=PRODUCT_RELATED_PRODUCT_CATEGORY('Flat Washer - M8',
'Flat Washer - M8',(#10422));
#10384=PRODUCT_RELATED_PRODUCT_CATEGORY('Hex Nut - M8','Hex Nut - M8',(#10423));
#10385=PRODUCT_RELATED_PRODUCT_CATEGORY('Bypass valve rotor',
'Bypass valve rotor',(#10424));
#10386=PRODUCT_RELATED_PRODUCT_CATEGORY('Ported ball','Ported ball',(#10425));
#10387=PRODUCT_RELATED_PRODUCT_CATEGORY('Stem','Stem',(#10426));
#10388=PRODUCT_RELATED_PRODUCT_CATEGORY('Lever','Lever',(#10427));
#10389=PRODUCT_RELATED_PRODUCT_CATEGORY('Lever keeper','Lever keeper',(#10428));
#10390=PRODUCT_RELATED_PRODUCT_CATEGORY('Bonded grip','Bonded grip',(#10429));
#10391=PRODUCT_RELATED_PRODUCT_CATEGORY('M4x10 Cap Screw',
'M4x10 Cap Screw',(#10430));
#10392=APPLICATION_PROTOCOL_DEFINITION('international standard',
'automotive_design',2009,#10393);
#10393=APPLICATION_CONTEXT(
'Core Data for Automotive Mechanical Design Process');
#10394=PRODUCT_CONTEXT('part definition',#10393,'mechanical');
#10395=PRODUCT('PAT-115','PAT-115',
'PAT-115',(#10394));
#10396=PRODUCT('Pipe loop union and valve body',
'Pipe loop union and valve body','Pipe loop union and valve body',(#10394));
#10397=PRODUCT('Bypass valve body','Bypass valve body',
'Bypass valve body',(#10394));
#10398=PRODUCT('Body inlet half','Body inlet half','Body inlet half',(#10394));
#10399=PRODUCT('Body outlet half','Body outlet half','Body outlet half',
(#10394));
#10400=PRODUCT('Split-body gasket','Split-body gasket',
'Split-body gasket',(#10394));
#10401=PRODUCT('Stem guide','Stem guide','Stem guide',(#10394));
#10402=PRODUCT('Packing ring','Packing ring','Packing ring',(#10394));
#10403=PRODUCT('Packing retainer','Packing retainer','Packing retainer',
(#10394));
#10404=PRODUCT('Lever stop bridge','Lever stop bridge',
'Lever stop bridge',(#10394));
#10405=PRODUCT('Ball seat','Ball seat','Ball seat',(#10394));
#10406=PRODUCT('M5x70 body screw','M5x70 body screw','M5x70 body screw',
(#10394));
#10407=PRODUCT('Flat Washer - M5','Flat Washer - M5','Flat Washer - M5',
(#10394));
#10408=PRODUCT('Hex Nut - M5','Hex Nut - M5','Hex Nut - M5',(#10394));
#10409=PRODUCT('Bridge spacer','Bridge spacer','Bridge spacer',(#10394));
#10410=PRODUCT('Cap Screw - M4x16','Cap Screw - M4x16',
'Cap Screw - M4x16',(#10394));
#10411=PRODUCT('Stop pin','Stop pin','Stop pin',(#10394));
#10412=PRODUCT('Union gasket','Union gasket','Union gasket',(#10394));
#10413=PRODUCT('Bypass tee','Bypass tee','Bypass tee',(#10394));
#10414=PRODUCT('Main-run pipe','Main-run pipe','Main-run pipe',(#10394));
#10415=PRODUCT('Bypass side pipe','Bypass side pipe','Bypass side pipe',
(#10394));
#10416=PRODUCT('Bypass valve pipe','Bypass valve pipe',
'Bypass valve pipe',(#10394));
#10417=PRODUCT('Pipe Elbow - 90 Degrees, 1-2 Inch Tapered Pipe Thread',
'Pipe Elbow - 90 Degrees, 1-2 Inch Tapered Pipe Thread',
'Pipe Elbow - 90 Degrees, 1-2 Inch Tapered Pipe Thread',(#10394));
#10418=PRODUCT('Hex Pipe Nipple - 1-2 Inch Tapered Pipe Thread',
'Hex Pipe Nipple - 1-2 Inch Tapered Pipe Thread',
'Hex Pipe Nipple - 1-2 Inch Tapered Pipe Thread',(#10394));
#10419=PRODUCT('Union half A','Union half A','Union half A',(#10394));
#10420=PRODUCT('Union half B','Union half B','Union half B',(#10394));
#10421=PRODUCT('Cap Screw - M8x30','Cap Screw - M8x30',
'Cap Screw - M8x30',(#10394));
#10422=PRODUCT('Flat Washer - M8','Flat Washer - M8','Flat Washer - M8',
(#10394));
#10423=PRODUCT('Hex Nut - M8','Hex Nut - M8','Hex Nut - M8',(#10394));
#10424=PRODUCT('Bypass valve rotor','Bypass valve rotor',
'Bypass valve rotor',(#10394));
#10425=PRODUCT('Ported ball','Ported ball','Ported ball',(#10394));
#10426=PRODUCT('Stem','Stem','Stem',(#10394));
#10427=PRODUCT('Lever','Lever','Lever',(#10394));
#10428=PRODUCT('Lever keeper','Lever keeper','Lever keeper',(#10394));
#10429=PRODUCT('Bonded grip','Bonded grip','Bonded grip',(#10394));
#10430=PRODUCT('M4x10 Cap Screw','M4x10 Cap Screw','M4x10 Cap Screw',(#10394));
#10431=PRESENTATION_STYLE_ASSIGNMENT((#10437));
#10432=PRESENTATION_STYLE_ASSIGNMENT((#10438));
#10433=PRESENTATION_STYLE_ASSIGNMENT((#10439));
#10434=PRESENTATION_STYLE_ASSIGNMENT((#10440));
#10435=PRESENTATION_STYLE_ASSIGNMENT((#10441));
#10436=PRESENTATION_STYLE_ASSIGNMENT((#10442));
#10437=SURFACE_STYLE_USAGE(.BOTH.,#10443);
#10438=SURFACE_STYLE_USAGE(.BOTH.,#10444);
#10439=SURFACE_STYLE_USAGE(.BOTH.,#10445);
#10440=SURFACE_STYLE_USAGE(.BOTH.,#10446);
#10441=SURFACE_STYLE_USAGE(.BOTH.,#10447);
#10442=SURFACE_STYLE_USAGE(.BOTH.,#10448);
#10443=SURFACE_SIDE_STYLE('',(#10449));
#10444=SURFACE_SIDE_STYLE('',(#10450));
#10445=SURFACE_SIDE_STYLE('',(#10451));
#10446=SURFACE_SIDE_STYLE('',(#10452));
#10447=SURFACE_SIDE_STYLE('',(#10453));
#10448=SURFACE_SIDE_STYLE('',(#10454));
#10449=SURFACE_STYLE_FILL_AREA(#10455);
#10450=SURFACE_STYLE_FILL_AREA(#10456);
#10451=SURFACE_STYLE_FILL_AREA(#10457);
#10452=SURFACE_STYLE_FILL_AREA(#10458);
#10453=SURFACE_STYLE_FILL_AREA(#10459);
#10454=SURFACE_STYLE_FILL_AREA(#10460);
#10455=FILL_AREA_STYLE('Steel - Satin',(#10461));
#10456=FILL_AREA_STYLE('CAD Library Painted - Engineering blue',(#10462));
#10457=FILL_AREA_STYLE('CAD Library Painted - Off white',(#10463));
#10458=FILL_AREA_STYLE('CAD Library Painted - Steel gray',(#10464));
#10459=FILL_AREA_STYLE('CAD Library Painted - Light blue',(#10465));
#10460=FILL_AREA_STYLE('CAD Library Painted - Graphite',(#10466));
#10461=FILL_AREA_STYLE_COLOUR('Steel - Satin',#10467);
#10462=FILL_AREA_STYLE_COLOUR('CAD Library Painted - Engineering blue',
#10468);
#10463=FILL_AREA_STYLE_COLOUR('CAD Library Painted - Off white',#10469);
#10464=FILL_AREA_STYLE_COLOUR('CAD Library Painted - Steel gray',#10470);
#10465=FILL_AREA_STYLE_COLOUR('CAD Library Painted - Light blue',#10471);
#10466=FILL_AREA_STYLE_COLOUR('CAD Library Painted - Graphite',#10472);
#10467=COLOUR_RGB('Steel - Satin',0.627450980392157,0.627450980392157,0.627450980392157);
#10468=COLOUR_RGB('CAD Library Painted - Engineering blue',0.12156862745098,
0.356862745098039,0.6);
#10469=COLOUR_RGB('CAD Library Painted - Off white',0.909803921568627,0.901960784313726,
0.858823529411765);
#10470=COLOUR_RGB('CAD Library Painted - Steel gray',0.592156862745098,
0.631372549019608,0.67843137254902);
#10471=COLOUR_RGB('CAD Library Painted - Light blue',0.286274509803922,
0.552941176470588,0.780392156862745);
#10472=COLOUR_RGB('CAD Library Painted - Graphite',0.0980392156862745,0.109803921568627,
0.125490196078431);
#10473=COLOUR_RGB('Dark Blue',0.08,0.2,0.34);
#10474=FILL_AREA_STYLE_COLOUR('',#10473);
#10475=FILL_AREA_STYLE('',(#10474));
#10476=SURFACE_STYLE_FILL_AREA(#10475);
#10477=SURFACE_SIDE_STYLE('',(#10476));
#10478=SURFACE_STYLE_USAGE(.BOTH.,#10477);
#10479=PRESENTATION_STYLE_ASSIGNMENT((#10478));
#10480=COLOUR_RGB('Light Blue',0.38,0.62,0.78);
#10481=FILL_AREA_STYLE_COLOUR('',#10480);
#10482=FILL_AREA_STYLE('',(#10481));
#10483=SURFACE_STYLE_FILL_AREA(#10482);
#10484=SURFACE_SIDE_STYLE('',(#10483));
#10485=SURFACE_STYLE_USAGE(.BOTH.,#10484);
#10486=PRESENTATION_STYLE_ASSIGNMENT((#10485));
#10487=COLOUR_RGB('Sky Blue',0.24,0.69,0.87);
#10488=FILL_AREA_STYLE_COLOUR('',#10487);
#10489=FILL_AREA_STYLE('',(#10488));
#10490=SURFACE_STYLE_FILL_AREA(#10489);
#10491=SURFACE_SIDE_STYLE('',(#10490));
#10492=SURFACE_STYLE_USAGE(.BOTH.,#10491);
#10493=PRESENTATION_STYLE_ASSIGNMENT((#10492));
#10494=COLOUR_RGB('Grey',0.48,0.52,0.57);
#10495=FILL_AREA_STYLE_COLOUR('',#10494);
#10496=FILL_AREA_STYLE('',(#10495));
#10497=SURFACE_STYLE_FILL_AREA(#10496);
#10498=SURFACE_SIDE_STYLE('',(#10497));
#10499=SURFACE_STYLE_USAGE(.BOTH.,#10498);
#10500=PRESENTATION_STYLE_ASSIGNMENT((#10499));
#10501=COLOUR_RGB('Black',0.12,0.14,0.17);
#10502=FILL_AREA_STYLE_COLOUR('',#10501);
#10503=FILL_AREA_STYLE('',(#10502));
#10504=SURFACE_STYLE_FILL_AREA(#10503);
#10505=SURFACE_SIDE_STYLE('',(#10504));
#10506=SURFACE_STYLE_USAGE(.BOTH.,#10505);
#10507=PRESENTATION_STYLE_ASSIGNMENT((#10506));
#10508=COLOUR_RGB('Off White',0.89,0.88,0.83);
#10509=FILL_AREA_STYLE_COLOUR('',#10508);
#10510=FILL_AREA_STYLE('',(#10509));
#10511=SURFACE_STYLE_FILL_AREA(#10510);
#10512=SURFACE_SIDE_STYLE('',(#10511));
#10513=SURFACE_STYLE_USAGE(.BOTH.,#10512);
#10514=PRESENTATION_STYLE_ASSIGNMENT((#10513));
ENDSEC;
END-ISO-10303-21;
